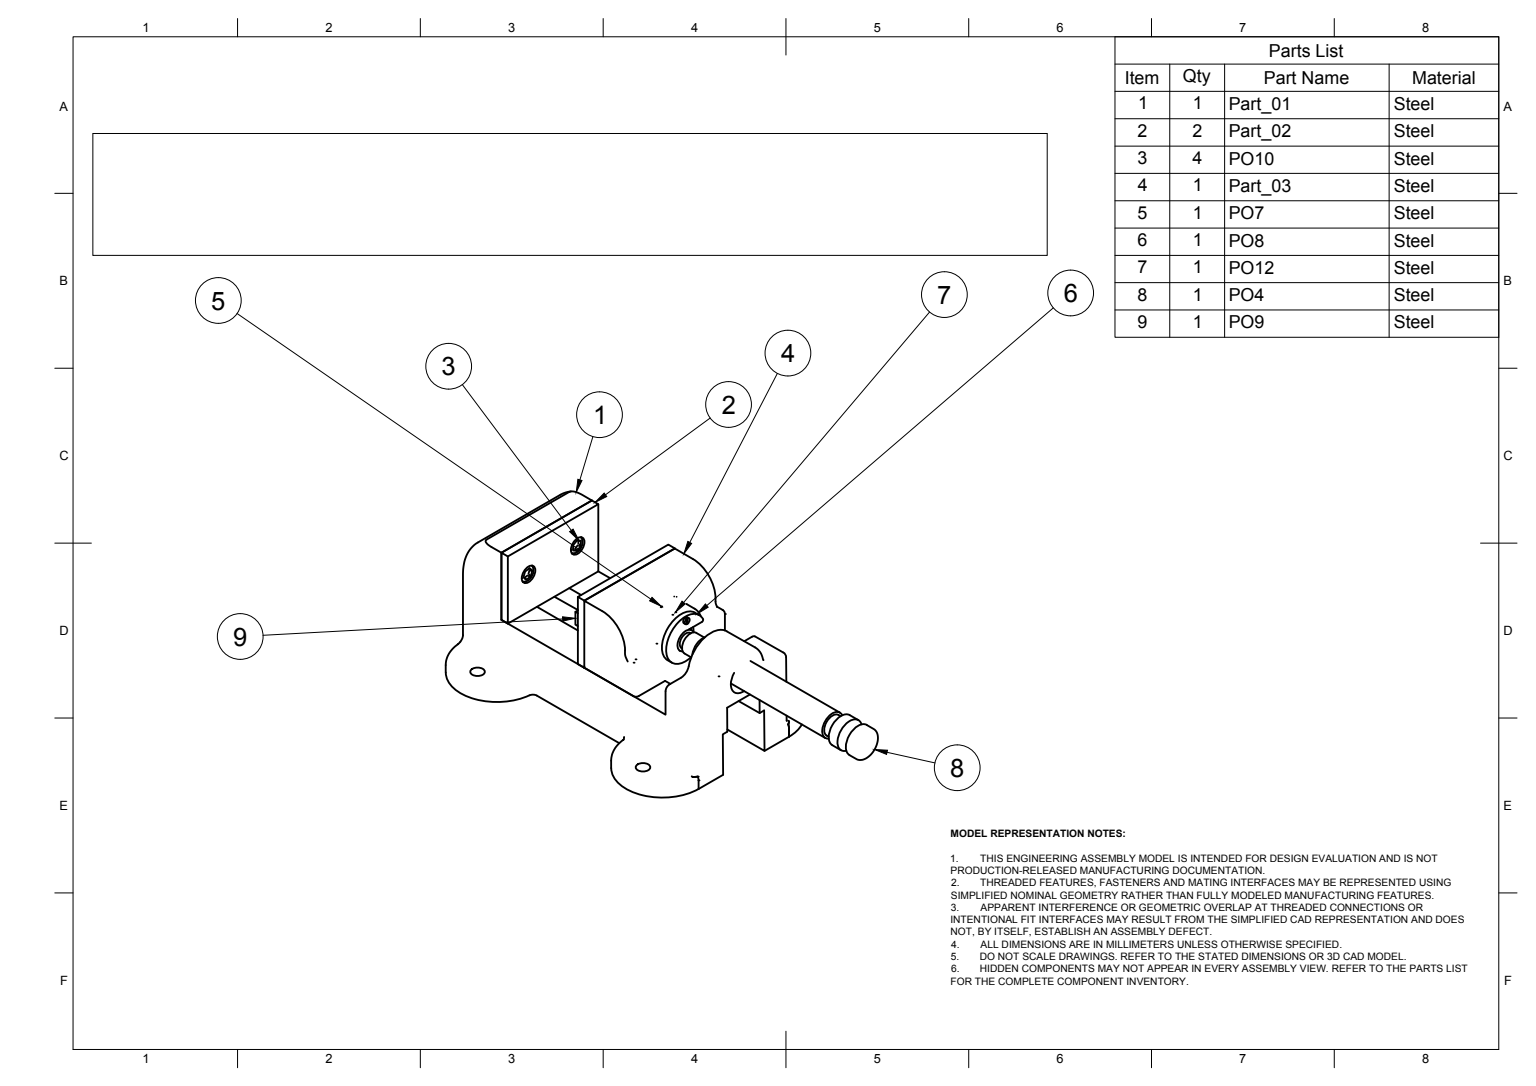
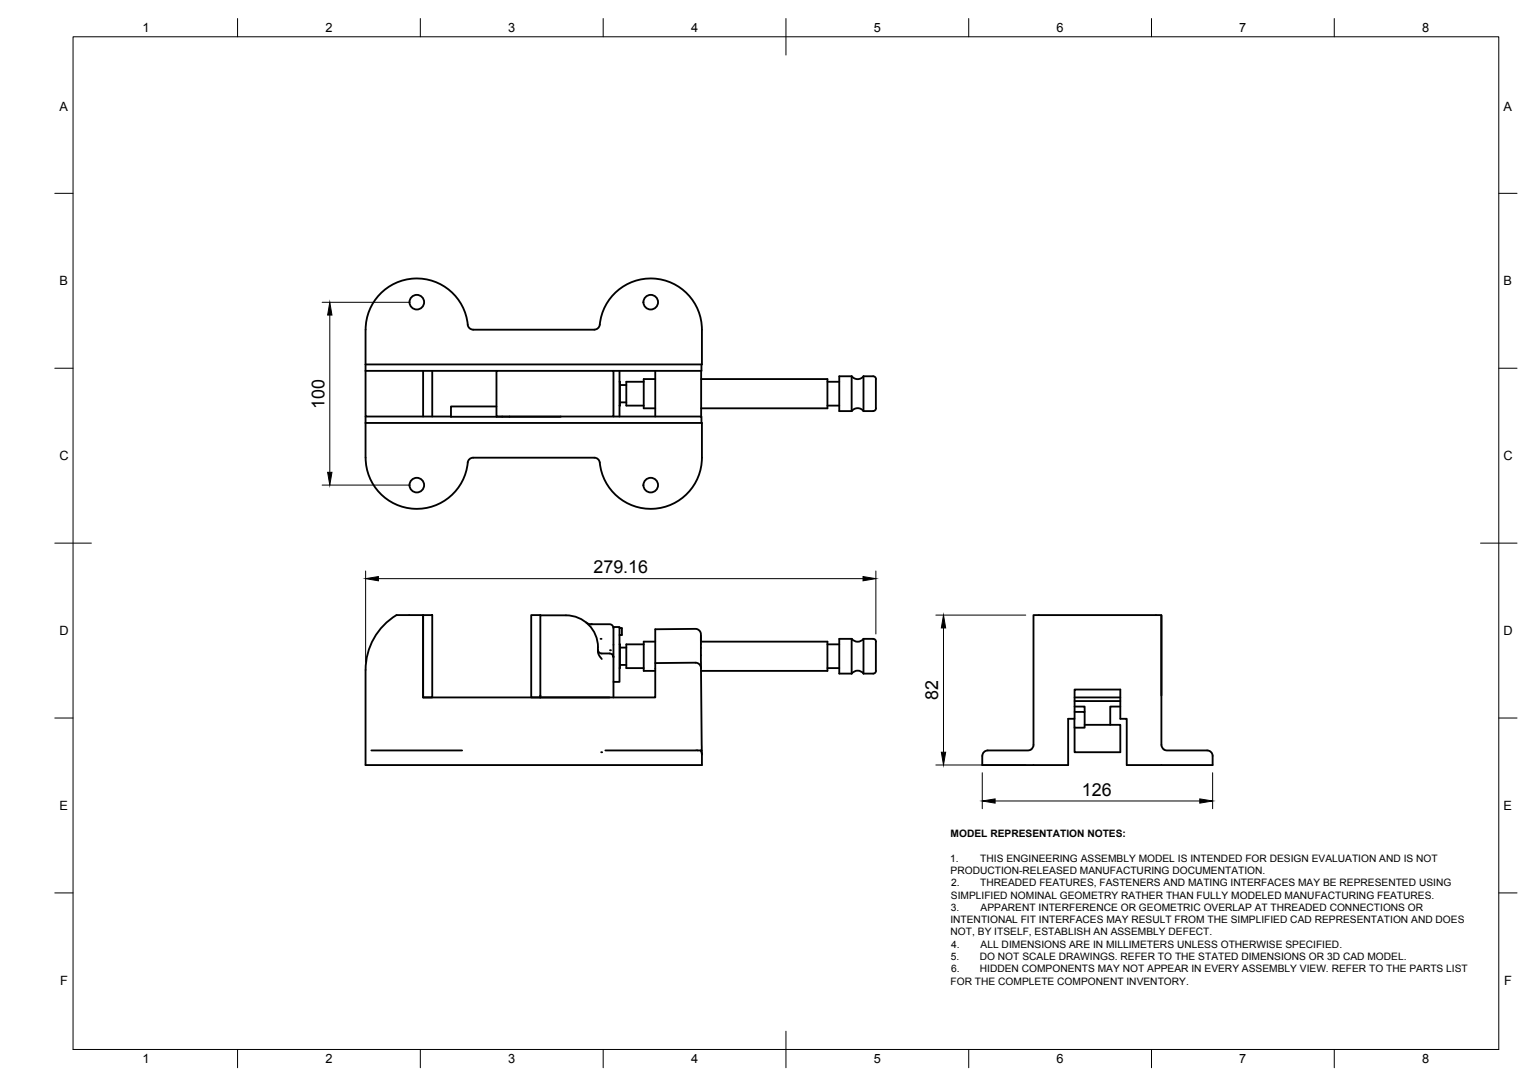
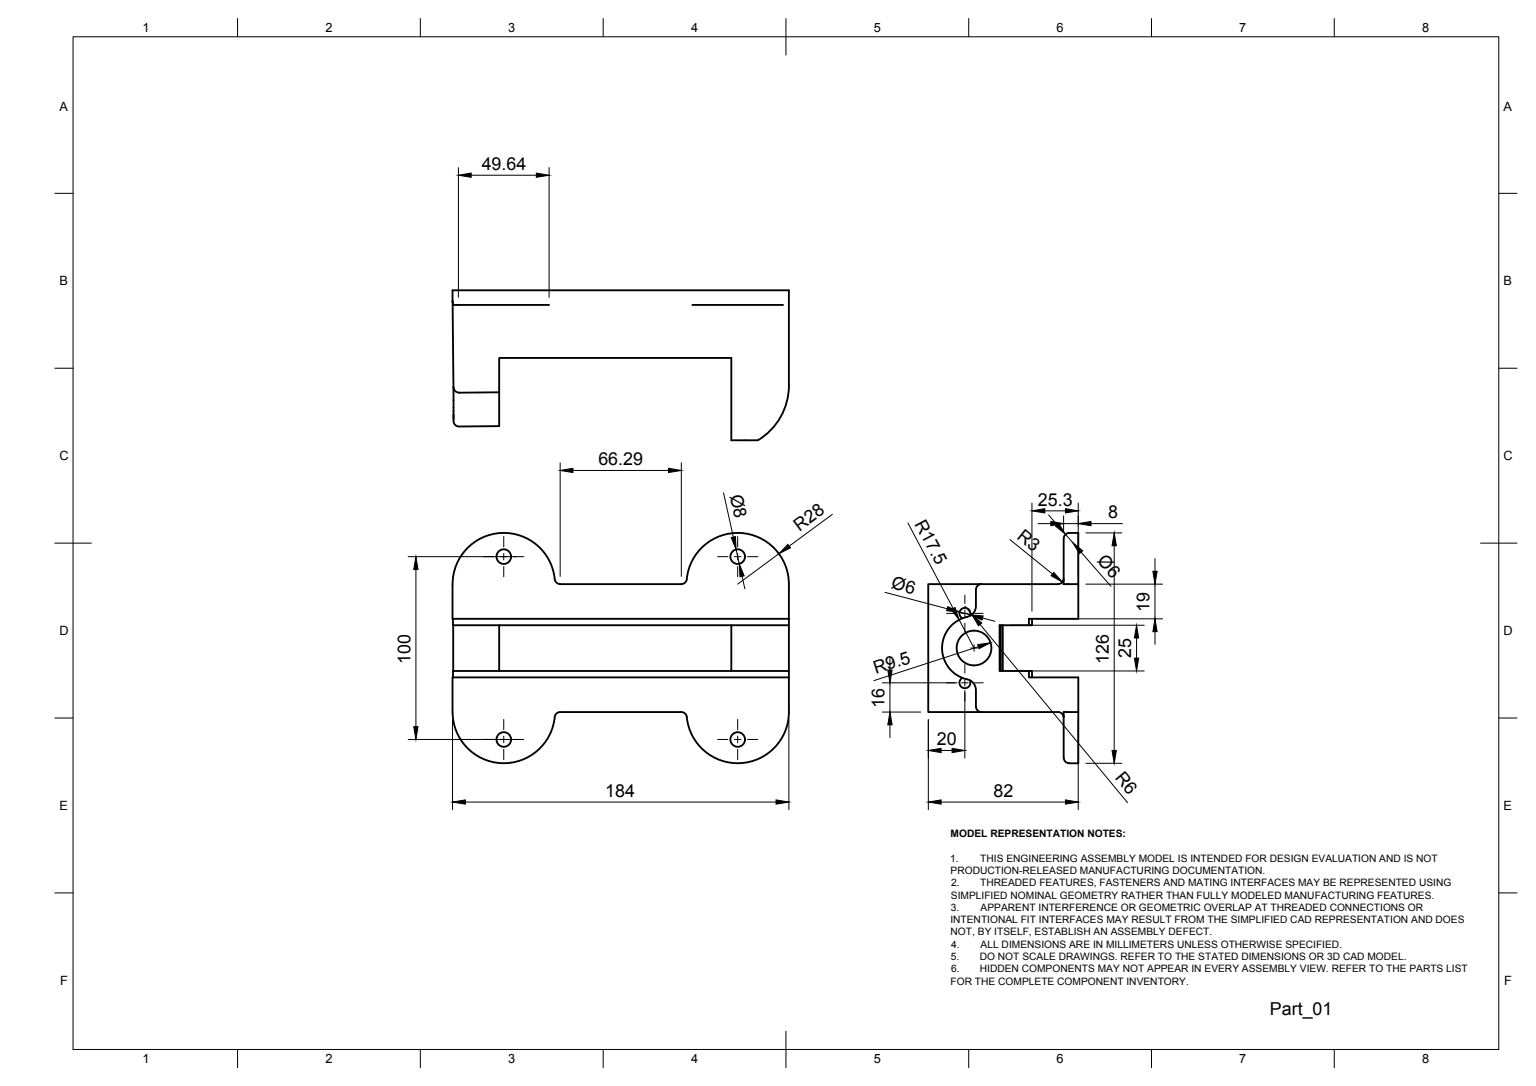
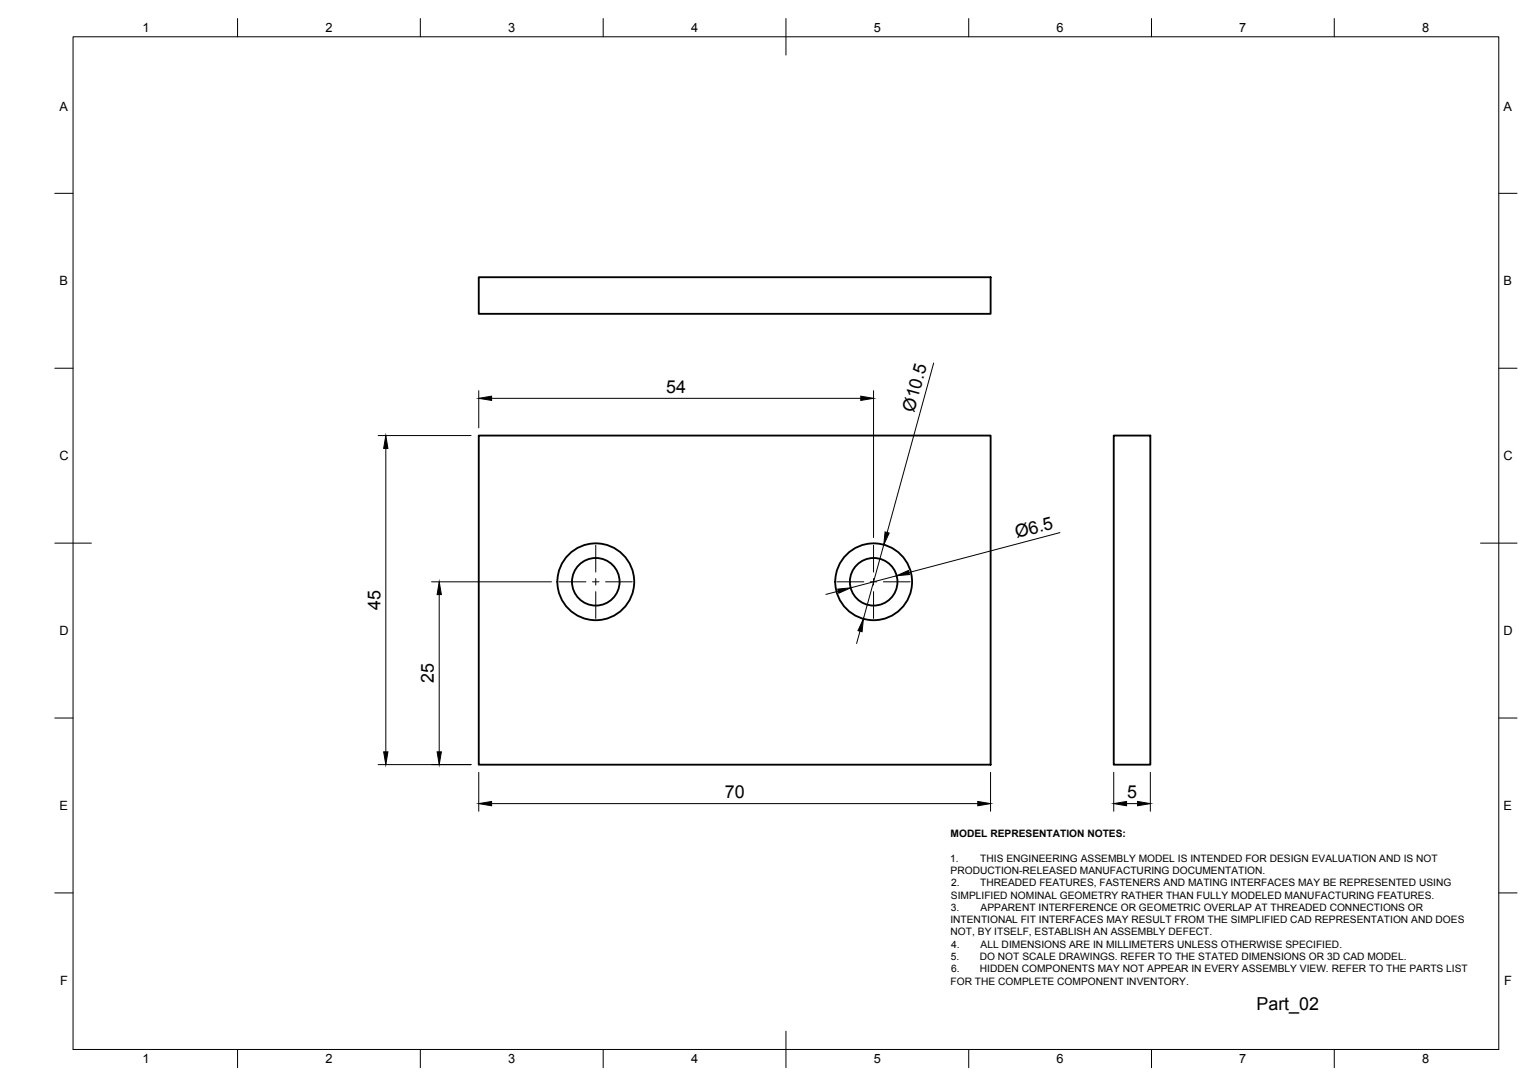
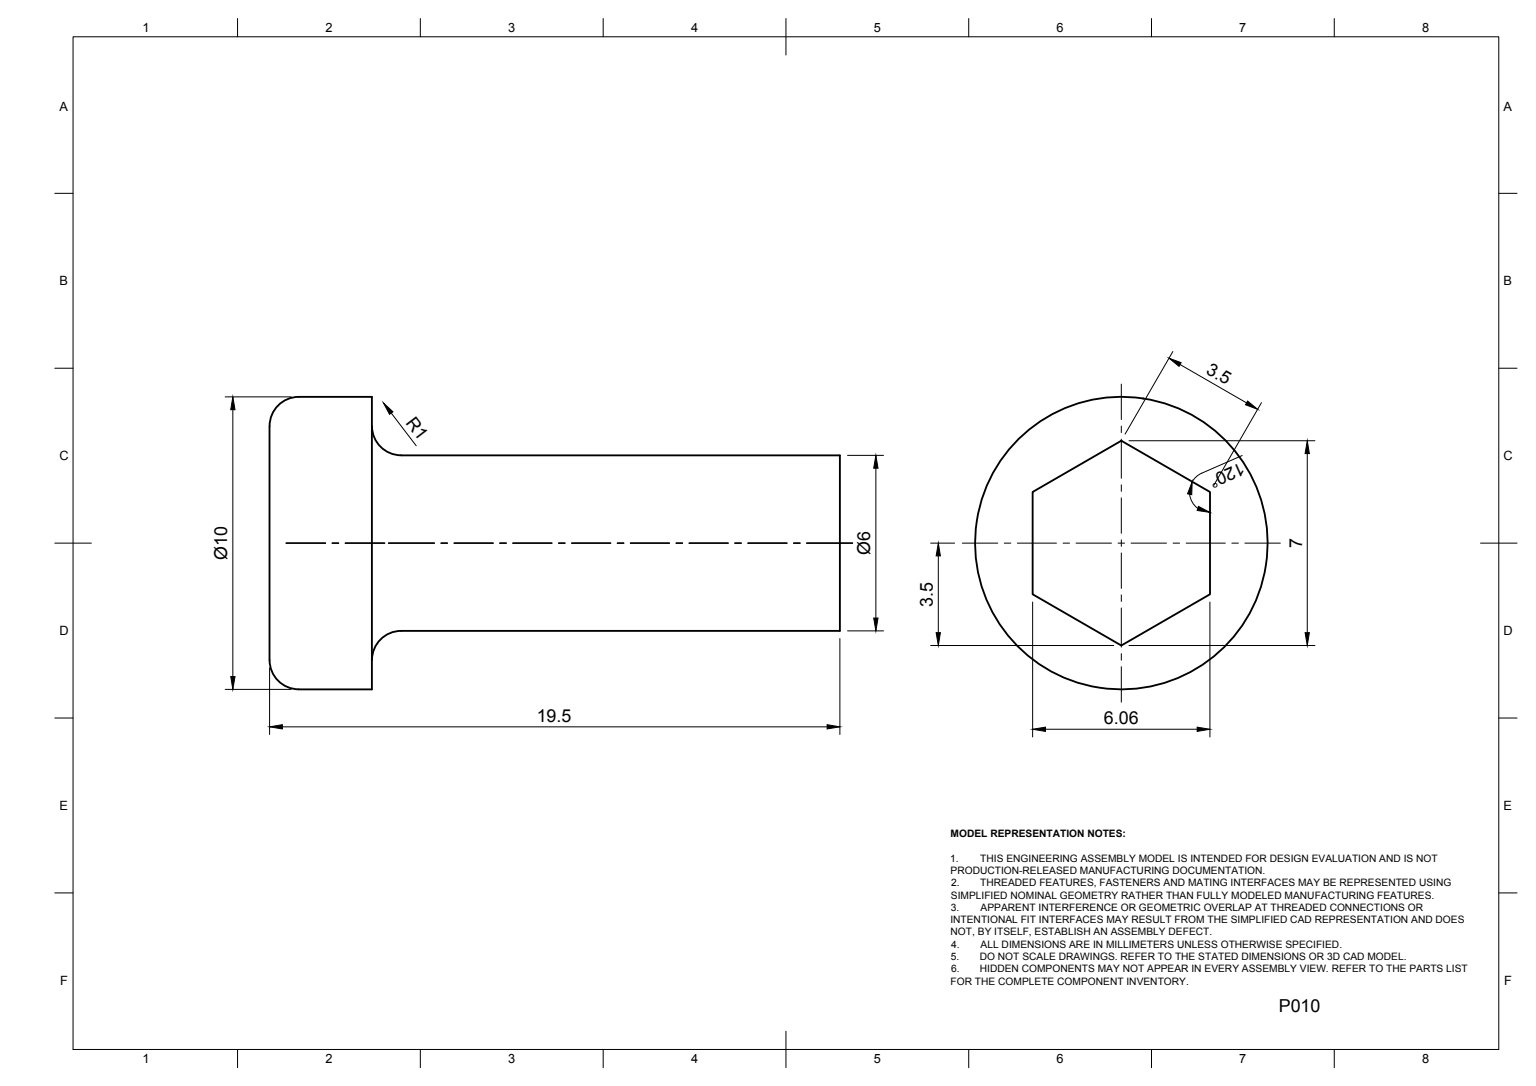
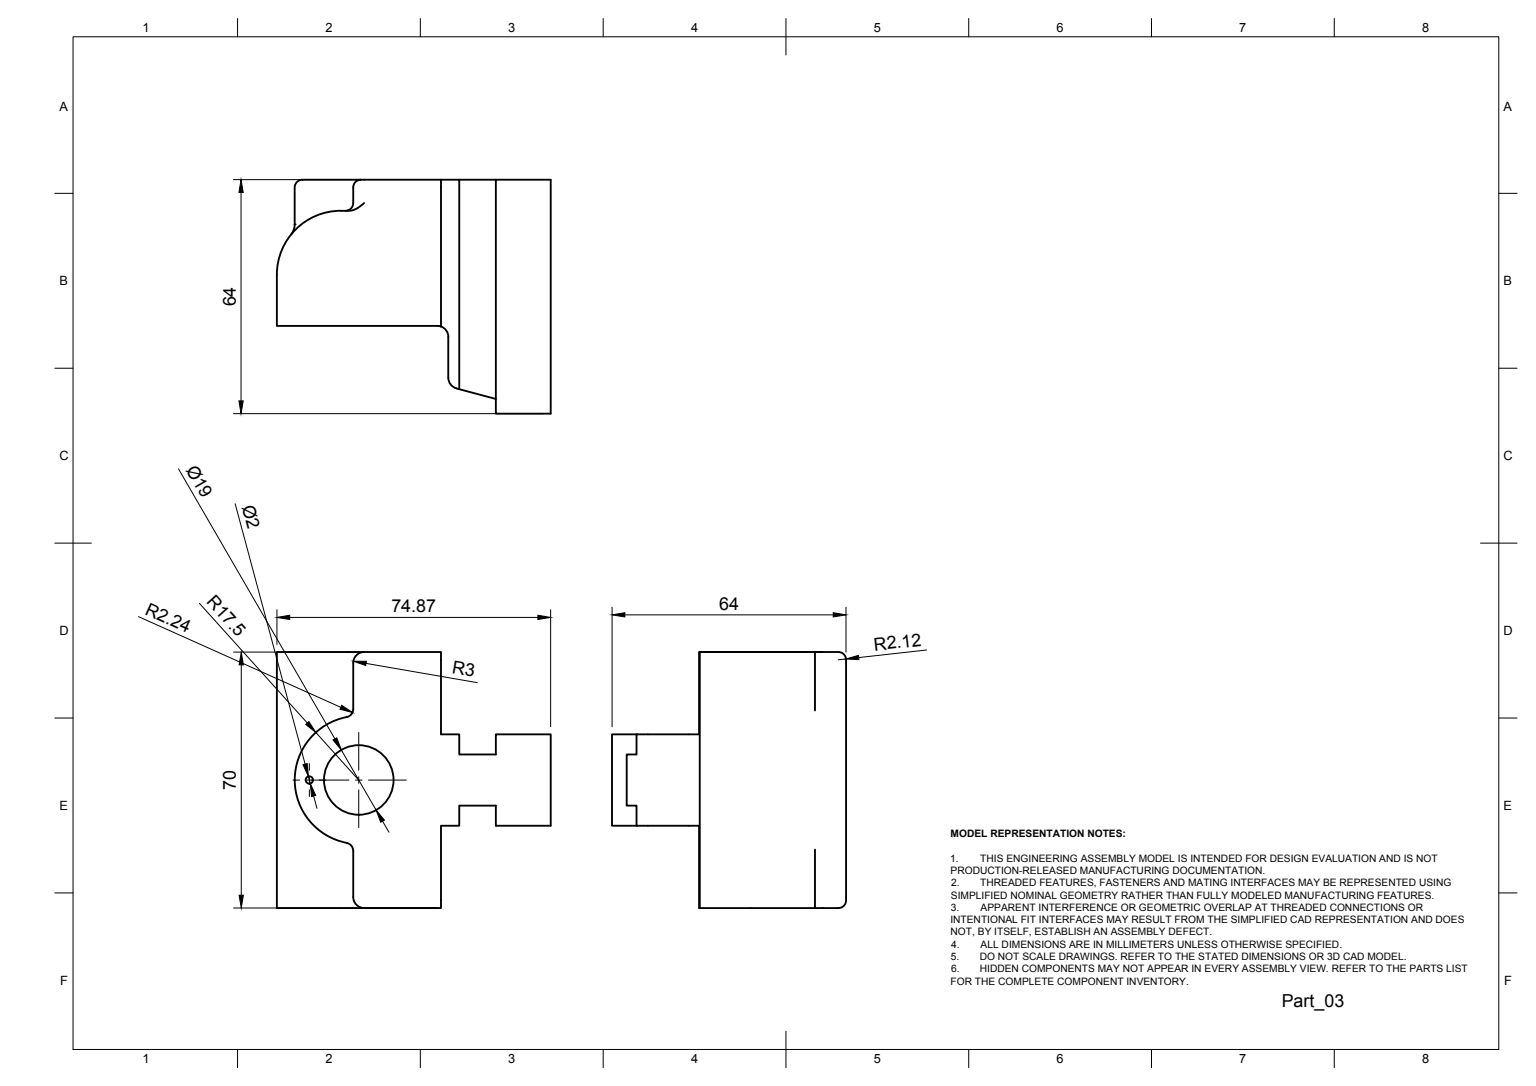
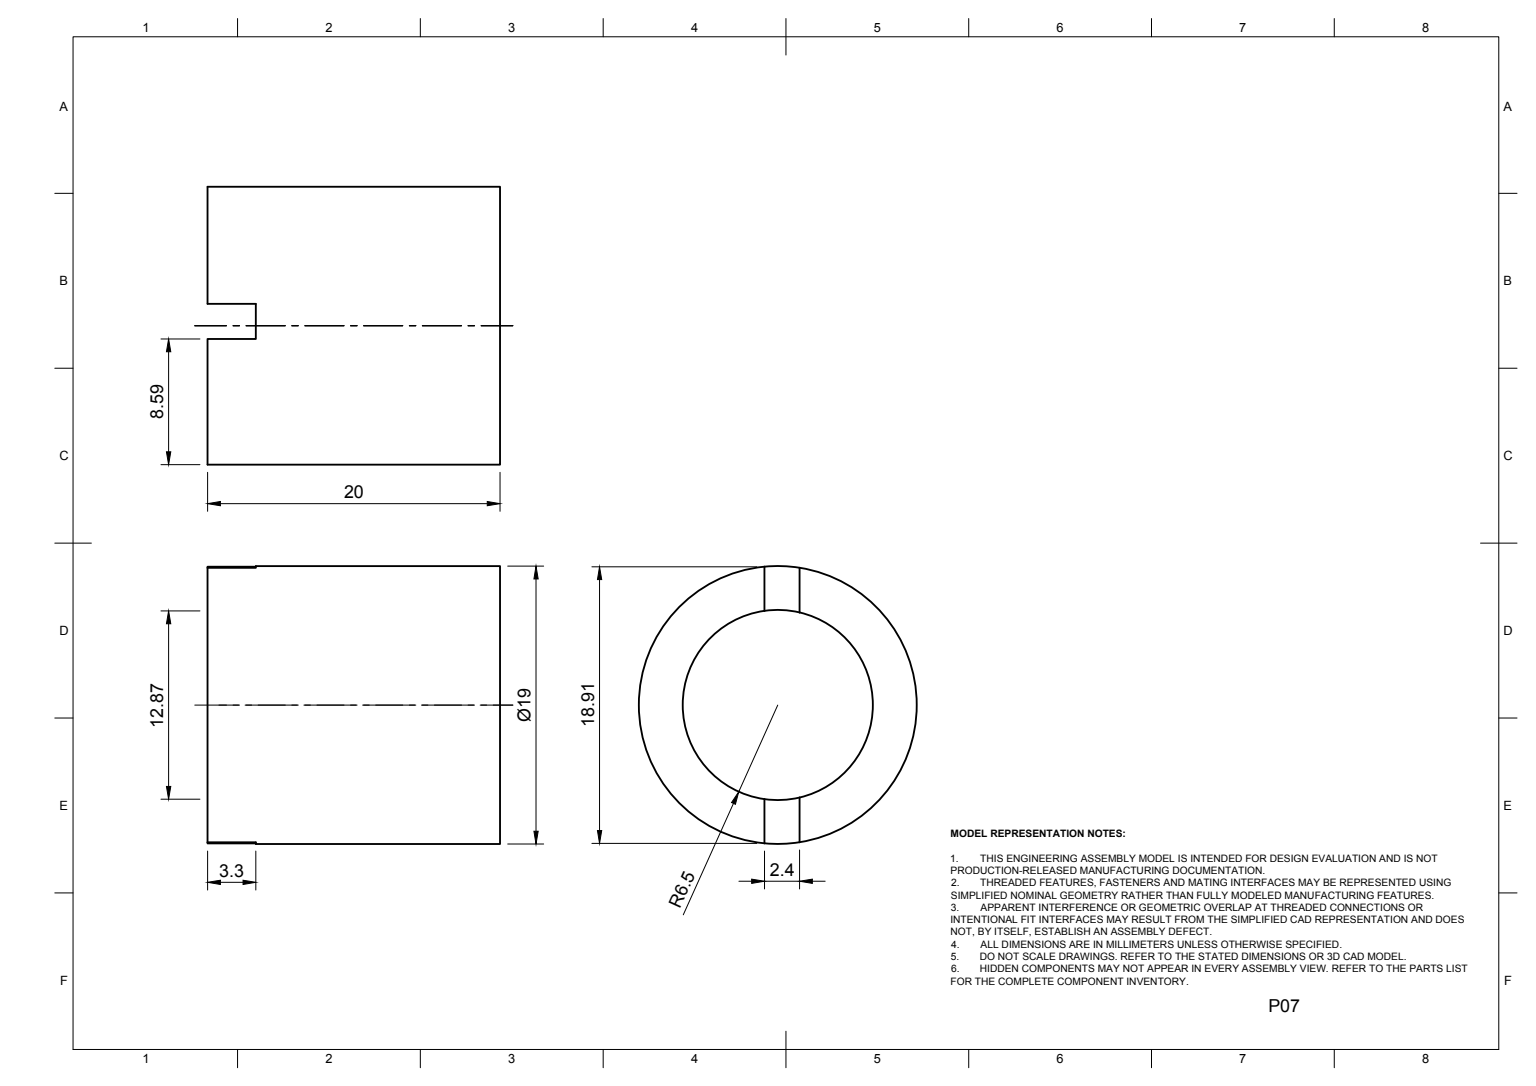
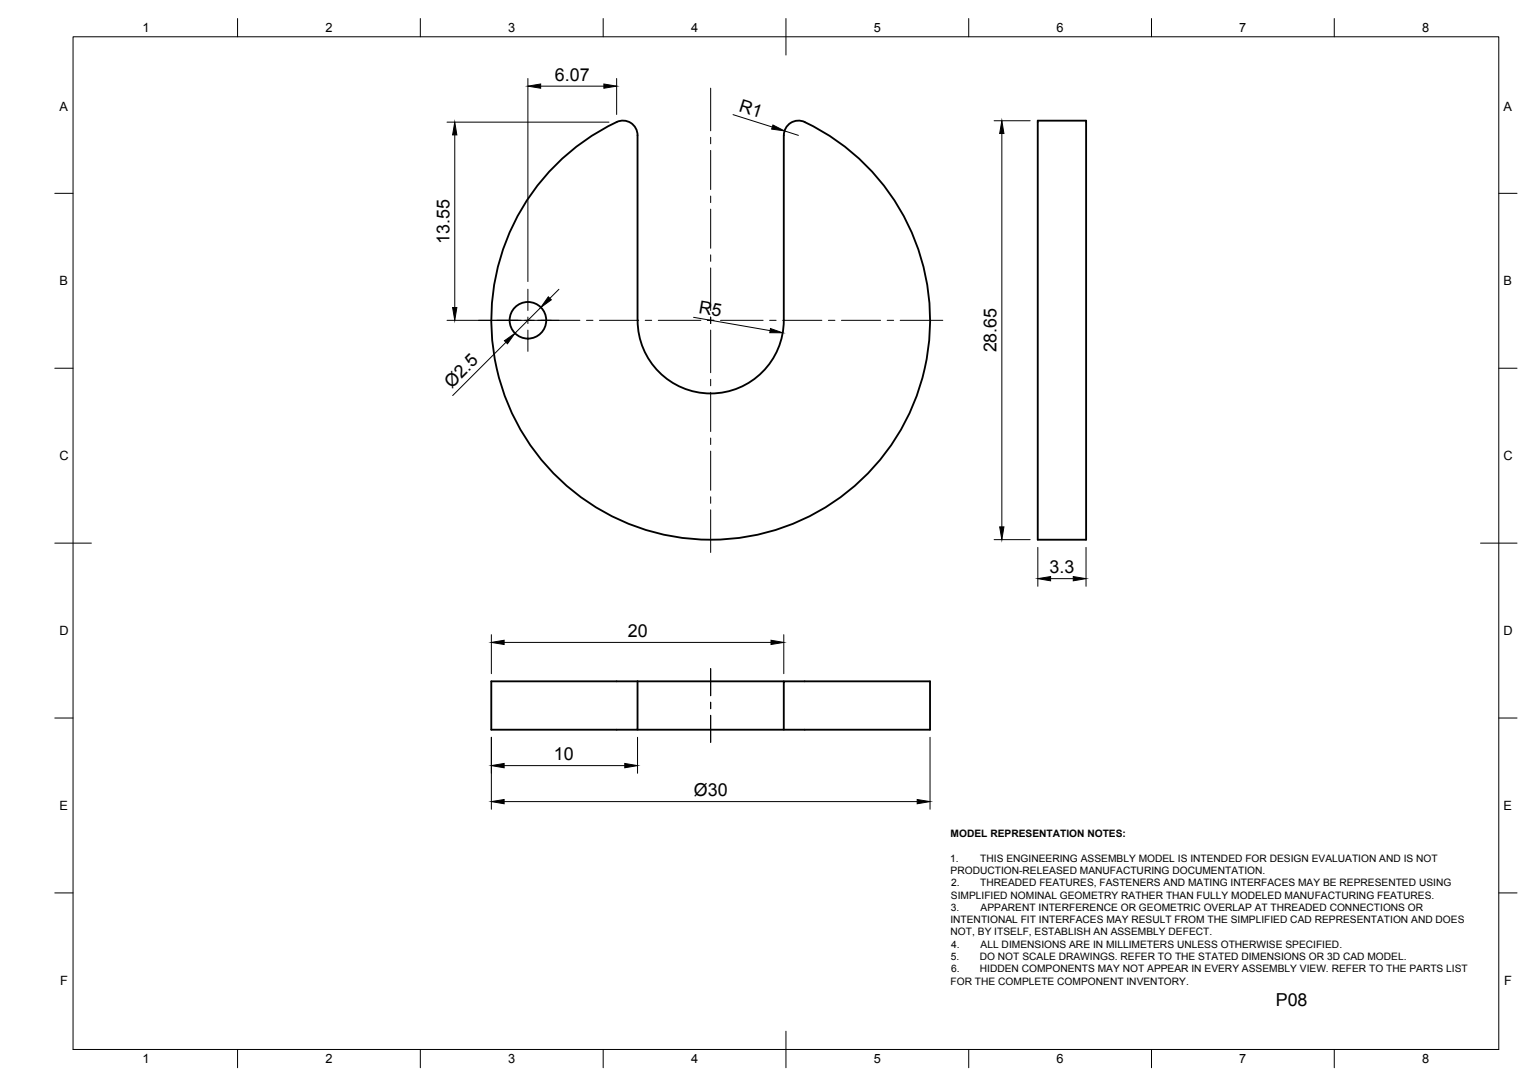
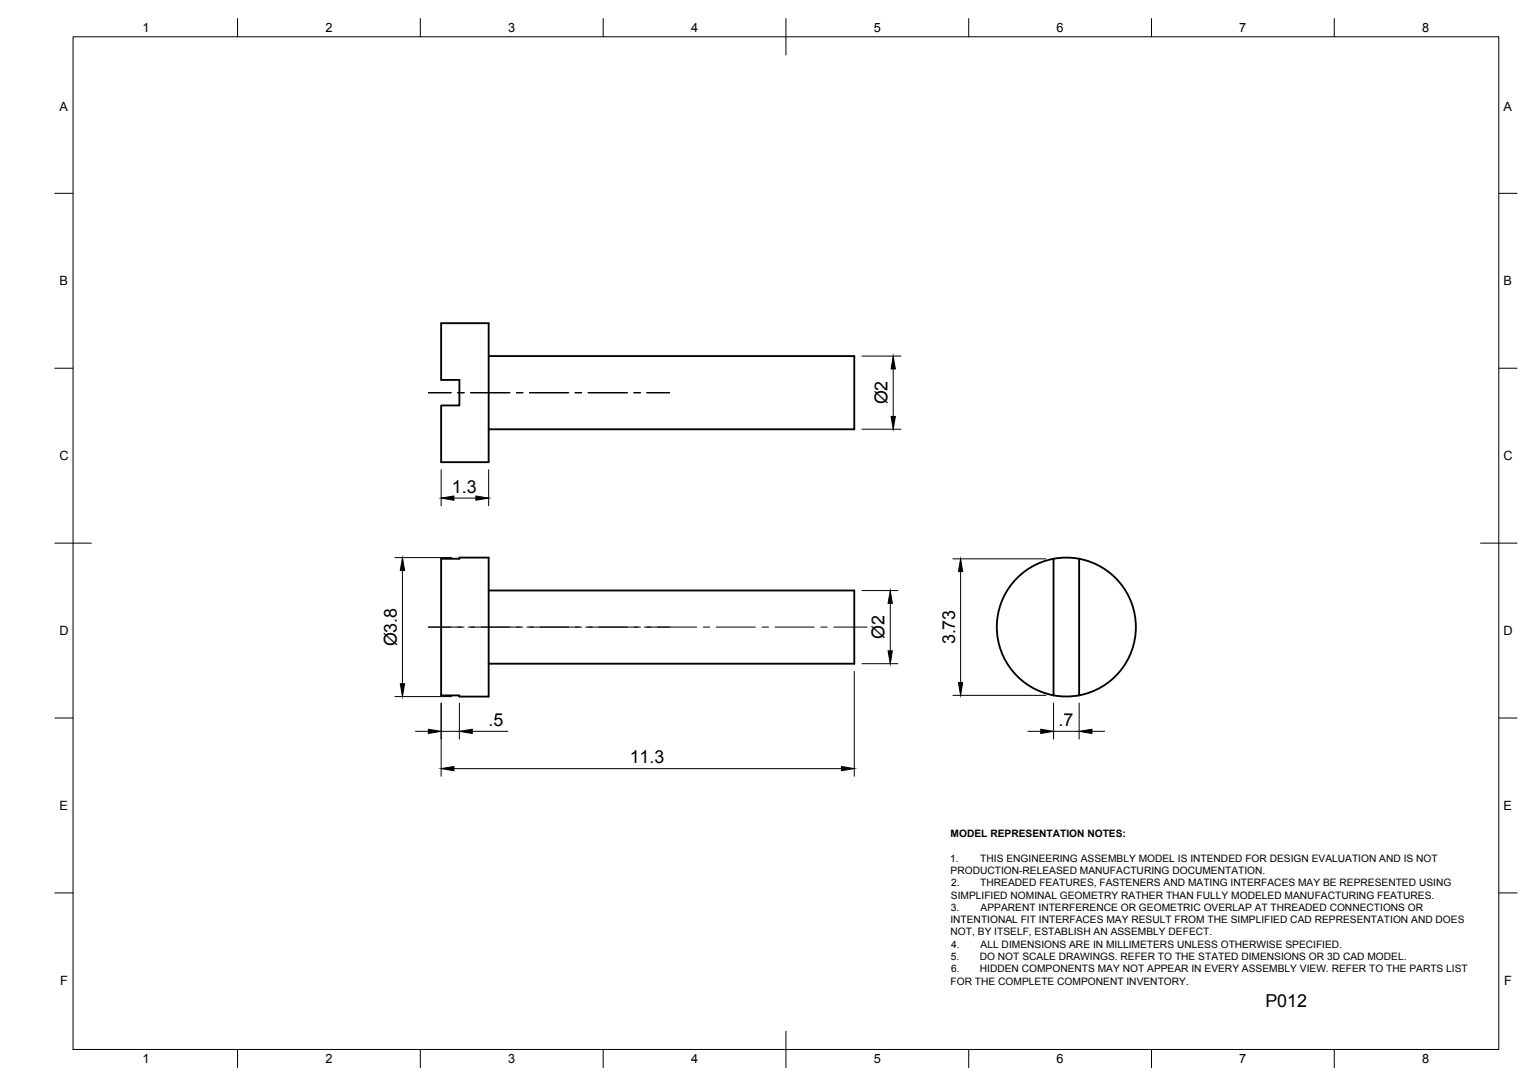
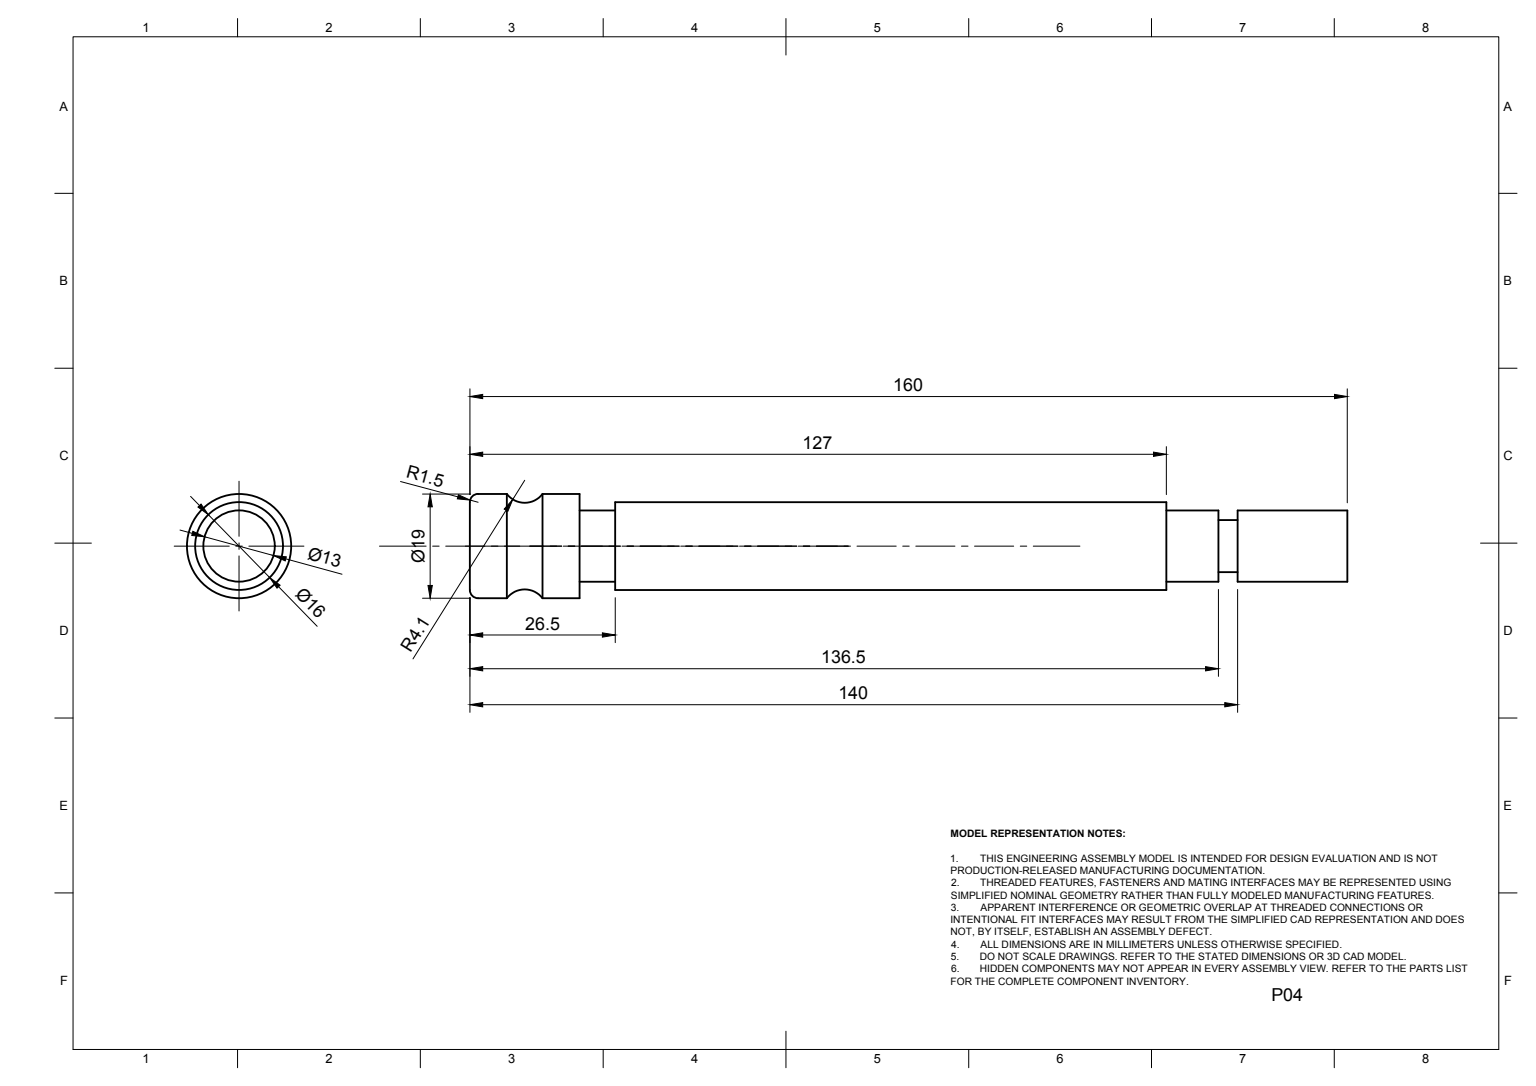
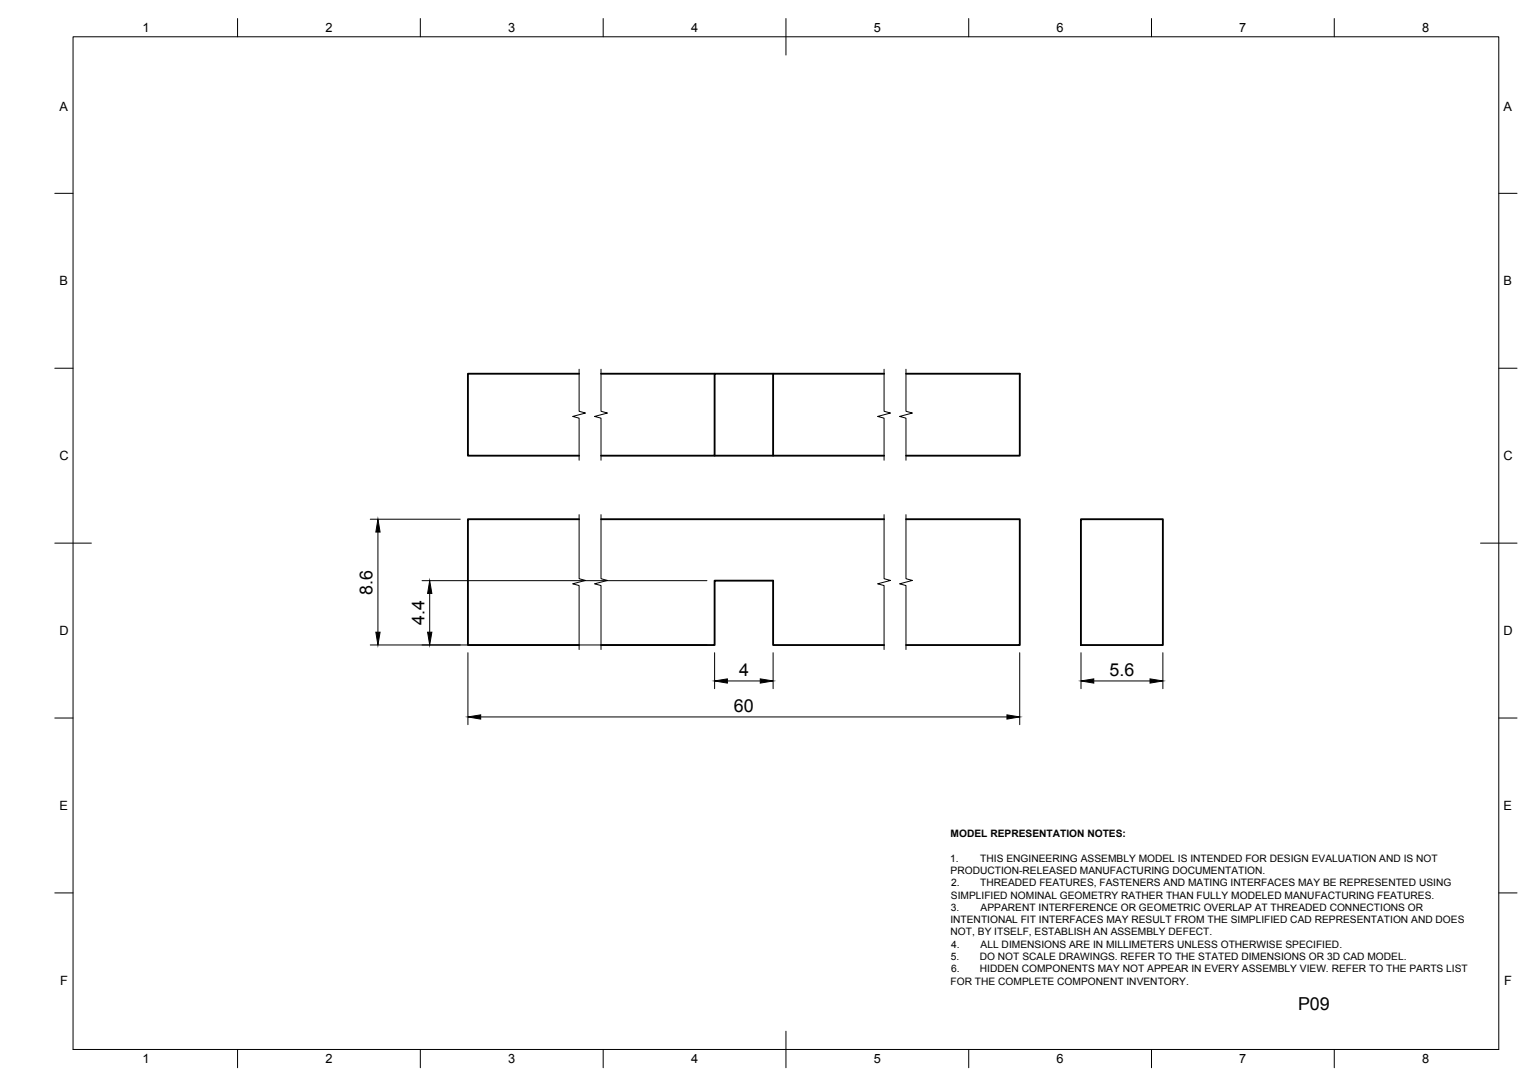
ISO-10303-21;
HEADER;
/* Generated by software containing ST-Developer
 * from STEP Tools, Inc. (www.steptools.com) 
 */

FILE_DESCRIPTION(
/* description */ (''),
/* implementation_level */ '2;1');

FILE_NAME(
/* name */ 'MAS-612',
/* time_stamp */ '2026-10-06T10:18:54-07:00',
/* author */ (''),
/* organization */ (''),
/* preprocessor_version */ 'ST-DEVELOPER v20.2',
/* originating_system */ 'Autodesk Translation Framework v15.15.0.0',
/* authorisation */ '');

FILE_SCHEMA (('AUTOMOTIVE_DESIGN { 1 0 10303 214 3 1 1 }'));
ENDSEC;

DATA;
#10=MECHANICAL_DESIGN_GEOMETRIC_PRESENTATION_REPRESENTATION('',(#81,#82,
#83,#84,#85,#86,#87,#88,#89),#8445);
#11=ITEM_DEFINED_TRANSFORMATION($,$,#4112,#4500);
#12=ITEM_DEFINED_TRANSFORMATION($,$,#4344,#4501);
#13=ITEM_DEFINED_TRANSFORMATION($,$,#4365,#4502);
#14=ITEM_DEFINED_TRANSFORMATION($,$,#4365,#4503);
#15=ITEM_DEFINED_TRANSFORMATION($,$,#4284,#4504);
#16=ITEM_DEFINED_TRANSFORMATION($,$,#4344,#4505);
#17=ITEM_DEFINED_TRANSFORMATION($,$,#4365,#4506);
#18=ITEM_DEFINED_TRANSFORMATION($,$,#4365,#4507);
#19=ITEM_DEFINED_TRANSFORMATION($,$,#4390,#4508);
#20=ITEM_DEFINED_TRANSFORMATION($,$,#4414,#4509);
#21=ITEM_DEFINED_TRANSFORMATION($,$,#4434,#4510);
#22=ITEM_DEFINED_TRANSFORMATION($,$,#4452,#4511);
#23=ITEM_DEFINED_TRANSFORMATION($,$,#4489,#4512);
#24=(
REPRESENTATION_RELATIONSHIP($,$,#8484,#8483)
REPRESENTATION_RELATIONSHIP_WITH_TRANSFORMATION(#11)
SHAPE_REPRESENTATION_RELATIONSHIP()
);
#25=(
REPRESENTATION_RELATIONSHIP($,$,#8486,#8483)
REPRESENTATION_RELATIONSHIP_WITH_TRANSFORMATION(#12)
SHAPE_REPRESENTATION_RELATIONSHIP()
);
#26=(
REPRESENTATION_RELATIONSHIP($,$,#8487,#8483)
REPRESENTATION_RELATIONSHIP_WITH_TRANSFORMATION(#13)
SHAPE_REPRESENTATION_RELATIONSHIP()
);
#27=(
REPRESENTATION_RELATIONSHIP($,$,#8487,#8483)
REPRESENTATION_RELATIONSHIP_WITH_TRANSFORMATION(#14)
SHAPE_REPRESENTATION_RELATIONSHIP()
);
#28=(
REPRESENTATION_RELATIONSHIP($,$,#8485,#8483)
REPRESENTATION_RELATIONSHIP_WITH_TRANSFORMATION(#15)
SHAPE_REPRESENTATION_RELATIONSHIP()
);
#29=(
REPRESENTATION_RELATIONSHIP($,$,#8486,#8483)
REPRESENTATION_RELATIONSHIP_WITH_TRANSFORMATION(#16)
SHAPE_REPRESENTATION_RELATIONSHIP()
);
#30=(
REPRESENTATION_RELATIONSHIP($,$,#8487,#8483)
REPRESENTATION_RELATIONSHIP_WITH_TRANSFORMATION(#17)
SHAPE_REPRESENTATION_RELATIONSHIP()
);
#31=(
REPRESENTATION_RELATIONSHIP($,$,#8487,#8483)
REPRESENTATION_RELATIONSHIP_WITH_TRANSFORMATION(#18)
SHAPE_REPRESENTATION_RELATIONSHIP()
);
#32=(
REPRESENTATION_RELATIONSHIP($,$,#8488,#8483)
REPRESENTATION_RELATIONSHIP_WITH_TRANSFORMATION(#19)
SHAPE_REPRESENTATION_RELATIONSHIP()
);
#33=(
REPRESENTATION_RELATIONSHIP($,$,#8489,#8483)
REPRESENTATION_RELATIONSHIP_WITH_TRANSFORMATION(#20)
SHAPE_REPRESENTATION_RELATIONSHIP()
);
#34=(
REPRESENTATION_RELATIONSHIP($,$,#8490,#8483)
REPRESENTATION_RELATIONSHIP_WITH_TRANSFORMATION(#21)
SHAPE_REPRESENTATION_RELATIONSHIP()
);
#35=(
REPRESENTATION_RELATIONSHIP($,$,#8491,#8483)
REPRESENTATION_RELATIONSHIP_WITH_TRANSFORMATION(#22)
SHAPE_REPRESENTATION_RELATIONSHIP()
);
#36=(
REPRESENTATION_RELATIONSHIP($,$,#8492,#8483)
REPRESENTATION_RELATIONSHIP_WITH_TRANSFORMATION(#23)
SHAPE_REPRESENTATION_RELATIONSHIP()
);
#37=CONTEXT_DEPENDENT_SHAPE_REPRESENTATION(#24,#8470);
#38=CONTEXT_DEPENDENT_SHAPE_REPRESENTATION(#25,#8471);
#39=CONTEXT_DEPENDENT_SHAPE_REPRESENTATION(#26,#8472);
#40=CONTEXT_DEPENDENT_SHAPE_REPRESENTATION(#27,#8473);
#41=CONTEXT_DEPENDENT_SHAPE_REPRESENTATION(#28,#8474);
#42=CONTEXT_DEPENDENT_SHAPE_REPRESENTATION(#29,#8475);
#43=CONTEXT_DEPENDENT_SHAPE_REPRESENTATION(#30,#8476);
#44=CONTEXT_DEPENDENT_SHAPE_REPRESENTATION(#31,#8477);
#45=CONTEXT_DEPENDENT_SHAPE_REPRESENTATION(#32,#8478);
#46=CONTEXT_DEPENDENT_SHAPE_REPRESENTATION(#33,#8479);
#47=CONTEXT_DEPENDENT_SHAPE_REPRESENTATION(#34,#8480);
#48=CONTEXT_DEPENDENT_SHAPE_REPRESENTATION(#35,#8481);
#49=CONTEXT_DEPENDENT_SHAPE_REPRESENTATION(#36,#8482);
#50=NEXT_ASSEMBLY_USAGE_OCCURRENCE('Configuration 1:1',
'Configuration 1:1','Configuration 1:1',#8494,#8495,'Configuration 1:1');
#51=NEXT_ASSEMBLY_USAGE_OCCURRENCE('Configuration 1:1',
'Configuration 1:1','Configuration 1:1',#8494,#8497,'Configuration 1:1');
#52=NEXT_ASSEMBLY_USAGE_OCCURRENCE('PO10:1','PO10:1','PO10:1',#8494,#8498,
'PO10:1');
#53=NEXT_ASSEMBLY_USAGE_OCCURRENCE('PO10:2','PO10:2','PO10:2',#8494,#8498,
'PO10:2');
#54=NEXT_ASSEMBLY_USAGE_OCCURRENCE('Configuration 1:1',
'Configuration 1:1','Configuration 1:1',#8494,#8496,'Configuration 1:1');
#55=NEXT_ASSEMBLY_USAGE_OCCURRENCE('Configuration 1:2',
'Configuration 1:2','Configuration 1:2',#8494,#8497,'Configuration 1:2');
#56=NEXT_ASSEMBLY_USAGE_OCCURRENCE('PO10:3','PO10:3','PO10:3',#8494,#8498,
'PO10:3');
#57=NEXT_ASSEMBLY_USAGE_OCCURRENCE('PO10:4','PO10:4','PO10:4',#8494,#8498,
'PO10:4');
#58=NEXT_ASSEMBLY_USAGE_OCCURRENCE('PO7:1','PO7:1','PO7:1',#8494,#8499,
'PO7:1');
#59=NEXT_ASSEMBLY_USAGE_OCCURRENCE('PO8:1','PO8:1','PO8:1',#8494,#8500,
'PO8:1');
#60=NEXT_ASSEMBLY_USAGE_OCCURRENCE('PO12:1','PO12:1','PO12:1',#8494,#8501,
'PO12:1');
#61=NEXT_ASSEMBLY_USAGE_OCCURRENCE('PO4:1','PO4:1','PO4:1',#8494,#8502,
'PO4:1');
#62=NEXT_ASSEMBLY_USAGE_OCCURRENCE('PO9:1','PO9:1','PO9:1',#8494,#8503,
'PO9:1');
#63=SHAPE_REPRESENTATION_RELATIONSHIP('SRR','None',#8484,#72);
#64=SHAPE_REPRESENTATION_RELATIONSHIP('SRR','None',#8485,#73);
#65=SHAPE_REPRESENTATION_RELATIONSHIP('SRR','None',#8486,#74);
#66=SHAPE_REPRESENTATION_RELATIONSHIP('SRR','None',#8487,#75);
#67=SHAPE_REPRESENTATION_RELATIONSHIP('SRR','None',#8488,#76);
#68=SHAPE_REPRESENTATION_RELATIONSHIP('SRR','None',#8489,#77);
#69=SHAPE_REPRESENTATION_RELATIONSHIP('SRR','None',#8490,#78);
#70=SHAPE_REPRESENTATION_RELATIONSHIP('SRR','None',#8491,#79);
#71=SHAPE_REPRESENTATION_RELATIONSHIP('SRR','None',#8492,#80);
#72=ADVANCED_BREP_SHAPE_REPRESENTATION('',(#90),#8436);
#73=ADVANCED_BREP_SHAPE_REPRESENTATION('',(#91),#8437);
#74=ADVANCED_BREP_SHAPE_REPRESENTATION('',(#92),#8438);
#75=ADVANCED_BREP_SHAPE_REPRESENTATION('',(#93),#8439);
#76=ADVANCED_BREP_SHAPE_REPRESENTATION('',(#94),#8440);
#77=ADVANCED_BREP_SHAPE_REPRESENTATION('',(#95),#8441);
#78=ADVANCED_BREP_SHAPE_REPRESENTATION('',(#96),#8442);
#79=ADVANCED_BREP_SHAPE_REPRESENTATION('',(#97),#8443);
#80=ADVANCED_BREP_SHAPE_REPRESENTATION('',(#98),#8444);
#81=STYLED_ITEM('',(#8537),#90);
#82=STYLED_ITEM('',(#8537),#91);
#83=STYLED_ITEM('',(#8537),#92);
#84=STYLED_ITEM('',(#8537),#93);
#85=STYLED_ITEM('',(#8537),#94);
#86=STYLED_ITEM('',(#8537),#95);
#87=STYLED_ITEM('',(#8537),#96);
#88=STYLED_ITEM('',(#8537),#97);
#89=STYLED_ITEM('',(#8537),#98);
#90=MANIFOLD_SOLID_BREP('Body1',#4002);
#91=MANIFOLD_SOLID_BREP('Body1',#4003);
#92=MANIFOLD_SOLID_BREP('Body1',#4004);
#93=MANIFOLD_SOLID_BREP('Body2',#4005);
#94=MANIFOLD_SOLID_BREP('Body1',#4006);
#95=MANIFOLD_SOLID_BREP('Body1',#4007);
#96=MANIFOLD_SOLID_BREP('Body1',#4008);
#97=MANIFOLD_SOLID_BREP('Body1',#4009);
#98=MANIFOLD_SOLID_BREP('Body1',#4010);
#99=CONICAL_SURFACE('',#4273,1.5,0.523598775598299);
#100=CONICAL_SURFACE('',#4276,1.5,0.523598775598299);
#101=CONICAL_SURFACE('',#4327,0.5,0.872664625997165);
#102=SPHERICAL_SURFACE('',#4234,3.);
#103=SPHERICAL_SURFACE('',#4236,3.);
#104=CYLINDRICAL_SURFACE('',#4148,3.);
#105=CYLINDRICAL_SURFACE('',#4152,3.);
#106=CYLINDRICAL_SURFACE('',#4156,3.);
#107=CYLINDRICAL_SURFACE('',#4162,3.);
#108=CYLINDRICAL_SURFACE('',#4177,3.);
#109=CYLINDRICAL_SURFACE('',#4178,28.);
#110=CYLINDRICAL_SURFACE('',#4187,28.);
#111=CYLINDRICAL_SURFACE('',#4202,3.);
#112=CYLINDRICAL_SURFACE('',#4203,3.);
#113=CYLINDRICAL_SURFACE('',#4210,3.);
#114=CYLINDRICAL_SURFACE('',#4216,3.);
#115=CYLINDRICAL_SURFACE('',#4230,3.);
#116=CYLINDRICAL_SURFACE('',#4232,3.);
#117=CYLINDRICAL_SURFACE('',#4238,28.);
#118=CYLINDRICAL_SURFACE('',#4240,3.);
#119=CYLINDRICAL_SURFACE('',#4243,5.99999999999999);
#120=CYLINDRICAL_SURFACE('',#4245,17.5);
#121=CYLINDRICAL_SURFACE('',#4247,5.99999999999999);
#122=CYLINDRICAL_SURFACE('',#4250,3.);
#123=CYLINDRICAL_SURFACE('',#4254,9.5);
#124=CYLINDRICAL_SURFACE('',#4258,3.);
#125=CYLINDRICAL_SURFACE('',#4260,3.);
#126=CYLINDRICAL_SURFACE('',#4263,3.);
#127=CYLINDRICAL_SURFACE('',#4264,4.);
#128=CYLINDRICAL_SURFACE('',#4266,28.);
#129=CYLINDRICAL_SURFACE('',#4268,4.);
#130=CYLINDRICAL_SURFACE('',#4269,3.99999999999999);
#131=CYLINDRICAL_SURFACE('',#4271,3.99999999999999);
#132=CYLINDRICAL_SURFACE('',#4275,3.);
#133=CYLINDRICAL_SURFACE('',#4278,3.);
#134=CYLINDRICAL_SURFACE('',#4281,35.);
#135=CYLINDRICAL_SURFACE('',#4285,3.);
#136=CYLINDRICAL_SURFACE('',#4289,3.);
#137=CYLINDRICAL_SURFACE('',#4294,17.5);
#138=CYLINDRICAL_SURFACE('',#4300,2.99999999999999);
#139=CYLINDRICAL_SURFACE('',#4302,2.23705055212463);
#140=CYLINDRICAL_SURFACE('',#4303,17.5);
#141=CYLINDRICAL_SURFACE('',#4304,2.23705055212463);
#142=CYLINDRICAL_SURFACE('',#4306,2.99999999999999);
#143=CYLINDRICAL_SURFACE('',#4315,3.00000000000001);
#144=CYLINDRICAL_SURFACE('',#4319,2.99999999999998);
#145=CYLINDRICAL_SURFACE('',#4329,1.);
#146=CYLINDRICAL_SURFACE('',#4331,9.5);
#147=CYLINDRICAL_SURFACE('',#4348,5.25);
#148=CYLINDRICAL_SURFACE('',#4350,3.25);
#149=CYLINDRICAL_SURFACE('',#4355,5.25);
#150=CYLINDRICAL_SURFACE('',#4357,3.25);
#151=CYLINDRICAL_SURFACE('',#4371,3.);
#152=CYLINDRICAL_SURFACE('',#4387,5.);
#153=CYLINDRICAL_SURFACE('',#4409,9.5);
#154=CYLINDRICAL_SURFACE('',#4411,6.5);
#155=CYLINDRICAL_SURFACE('',#4415,1.25);
#156=CYLINDRICAL_SURFACE('',#4418,5.00000007450581);
#157=CYLINDRICAL_SURFACE('',#4422,0.999999999999998);
#158=CYLINDRICAL_SURFACE('',#4425,15.);
#159=CYLINDRICAL_SURFACE('',#4428,1.);
#160=CYLINDRICAL_SURFACE('',#4445,1.);
#161=CYLINDRICAL_SURFACE('',#4449,1.9);
#162=CYLINDRICAL_SURFACE('',#4458,9.5);
#163=CYLINDRICAL_SURFACE('',#4466,9.5);
#164=CYLINDRICAL_SURFACE('',#4470,6.5);
#165=CYLINDRICAL_SURFACE('',#4475,6.50000009685755);
#166=CYLINDRICAL_SURFACE('',#4478,4.75);
#167=CYLINDRICAL_SURFACE('',#4480,6.5);
#168=CYLINDRICAL_SURFACE('',#4484,8.);
#169=ELLIPSE('',#4142,6.70820393249937,3.);
#170=ELLIPSE('',#4143,6.70820393249937,3.);
#171=ELLIPSE('',#4171,6.70820393249937,3.);
#172=ELLIPSE('',#4172,6.70820393249937,3.);
#173=ELLIPSE('',#4180,6.70820393249938,3.);
#174=ELLIPSE('',#4181,6.70820393249937,3.);
#175=ELLIPSE('',#4191,3.00051436158052,3.);
#176=ELLIPSE('',#4193,6.00025719732504,6.);
#177=ELLIPSE('',#4200,6.70820393249937,3.);
#178=ELLIPSE('',#4201,6.70820393249938,3.);
#179=ELLIPSE('',#4204,3.00051436158052,3.);
#180=ELLIPSE('',#4208,6.00025719732504,6.);
#181=ELLIPSE('',#4218,6.0005786784788,5.99999999999999);
#182=ELLIPSE('',#4220,9.00038579598755,8.99999999999999);
#183=ELLIPSE('',#4222,14.5006215602022,14.5);
#184=ELLIPSE('',#4223,17.5005150104847,17.5);
#185=ELLIPSE('',#4224,9.00038579598755,8.99999999999999);
#186=ELLIPSE('',#4225,6.0005786784788,5.99999999999999);
#187=ELLIPSE('',#4241,3.00012859866252,3.);
#188=ELLIPSE('',#4244,6.00025719732503,5.99999999999999);
#189=ELLIPSE('',#4246,17.5007501588647,17.5);
#190=ELLIPSE('',#4248,6.00025719732503,5.99999999999999);
#191=ELLIPSE('',#4251,3.00012859866252,3.);
#192=ELLIPSE('',#4255,9.50040722909798,9.5);
#193=TOROIDAL_SURFACE('',#4137,25.,3.);
#194=TOROIDAL_SURFACE('',#4144,32.,3.);
#195=TOROIDAL_SURFACE('',#4150,6.,3.);
#196=TOROIDAL_SURFACE('',#4158,32.,3.);
#197=TOROIDAL_SURFACE('',#4166,25.,3.);
#198=TOROIDAL_SURFACE('',#4173,6.,3.);
#199=TOROIDAL_SURFACE('',#4183,25.,3.);
#200=TOROIDAL_SURFACE('',#4194,25.,3.);
#201=TOROIDAL_SURFACE('',#4212,8.99999999999999,3.);
#202=TOROIDAL_SURFACE('',#4226,8.99999999999999,3.);
#203=TOROIDAL_SURFACE('',#4366,4.,1.);
#204=TOROIDAL_SURFACE('',#4382,4.,1.);
#205=TOROIDAL_SURFACE('',#4453,8.,1.5);
#206=TOROIDAL_SURFACE('',#4462,12.0000001788139,4.1);
#207=B_SPLINE_CURVE_WITH_KNOTS('',3,(#5747,#5748,#5749,#5750),
 .UNSPECIFIED.,.F.,.F.,(4,4),(-0.314873215025081,0.),.UNSPECIFIED.);
#208=B_SPLINE_CURVE_WITH_KNOTS('',3,(#5753,#5754,#5755,#5756),
 .UNSPECIFIED.,.F.,.F.,(4,4),(0.,0.314873215025081),.UNSPECIFIED.);
#209=B_SPLINE_CURVE_WITH_KNOTS('',3,(#5784,#5785,#5786,#5787),
 .UNSPECIFIED.,.F.,.F.,(4,4),(-0.0585005125063144,0.),.UNSPECIFIED.);
#210=B_SPLINE_CURVE_WITH_KNOTS('',3,(#5790,#5791,#5792,#5793),
 .UNSPECIFIED.,.F.,.F.,(4,4),(0.,0.0585005125063144),.UNSPECIFIED.);
#211=B_SPLINE_CURVE_WITH_KNOTS('',3,(#5835,#5836,#5837,#5838,#5839,#5840,
#5841,#5842,#5843,#5844,#5845,#5846,#5847,#5848),.UNSPECIFIED.,.F.,.F.,
(4,2,2,2,2,2,4),(1.81481027575948,1.85509507173471,1.89964280797494,2.0220220083772,
2.21769356951572,2.39982278968484,2.58195200985395),.UNSPECIFIED.);
#212=B_SPLINE_CURVE_WITH_KNOTS('',3,(#5887,#5888,#5889,#5890,#5891,#5892,
#5893,#5894,#5895,#5896,#5897,#5898,#5899,#5900),.UNSPECIFIED.,.F.,.F.,
(4,2,2,2,2,2,4),(4.67728909318397,4.85941831335309,5.04154753352221,5.23721909466073,
5.35959829506298,5.40414603130322,5.44443082727844),.UNSPECIFIED.);
#213=B_SPLINE_CURVE_WITH_KNOTS('',3,(#5933,#5934,#5935,#5936),
 .UNSPECIFIED.,.F.,.F.,(4,4),(-0.31487081906698,0.),.UNSPECIFIED.);
#214=B_SPLINE_CURVE_WITH_KNOTS('',3,(#5938,#5939,#5940,#5941),
 .UNSPECIFIED.,.F.,.F.,(4,4),(0.,0.31487081906698),.UNSPECIFIED.);
#215=B_SPLINE_CURVE_WITH_KNOTS('',3,(#5971,#5972,#5973,#5974),
 .UNSPECIFIED.,.F.,.F.,(4,4),(-0.0585005125063158,0.),.UNSPECIFIED.);
#216=B_SPLINE_CURVE_WITH_KNOTS('',3,(#5975,#5976,#5977,#5978),
 .UNSPECIFIED.,.F.,.F.,(4,4),(0.,0.0585005125063158),.UNSPECIFIED.);
#217=B_SPLINE_CURVE_WITH_KNOTS('',3,(#6078,#6079,#6080,#6081),
 .UNSPECIFIED.,.F.,.F.,(4,4),(-0.0585005125063147,0.),.UNSPECIFIED.);
#218=B_SPLINE_CURVE_WITH_KNOTS('',3,(#6084,#6085,#6086,#6087),
 .UNSPECIFIED.,.F.,.F.,(4,4),(0.,0.0585005125063147),.UNSPECIFIED.);
#219=B_SPLINE_CURVE_WITH_KNOTS('',3,(#6121,#6122,#6123,#6124,#6125,#6126),
 .UNSPECIFIED.,.F.,.F.,(4,2,4),(0.058804296831916,0.150601760228585,0.290945138364171),
 .UNSPECIFIED.);
#220=B_SPLINE_CURVE_WITH_KNOTS('',3,(#6127,#6128,#6129,#6130,#6131),
 .UNSPECIFIED.,.F.,.F.,(4,1,4),(0.937613435458313,0.988925248429188,1.25041151877174),
 .UNSPECIFIED.);
#221=B_SPLINE_CURVE_WITH_KNOTS('',3,(#6133,#6134,#6135,#6136),
 .UNSPECIFIED.,.F.,.F.,(4,4),(-1.25041151877174,-1.10394303083322),
 .UNSPECIFIED.);
#222=B_SPLINE_CURVE_WITH_KNOTS('',3,(#6138,#6139,#6140,#6141,#6142,#6143),
 .UNSPECIFIED.,.F.,.F.,(4,2,4),(-0.00122772925122373,0.,0.0713282894365937),
 .UNSPECIFIED.);
#223=B_SPLINE_CURVE_WITH_KNOTS('',3,(#6144,#6145,#6146,#6147,#6148,#6149),
 .UNSPECIFIED.,.F.,.F.,(4,2,4),(0.104979741457986,0.218385659282761,0.376958276855987),
 .UNSPECIFIED.);
#224=B_SPLINE_CURVE_WITH_KNOTS('',3,(#6160,#6161,#6162,#6163,#6164,#6165),
 .UNSPECIFIED.,.F.,.F.,(4,2,4),(0.377503618079906,0.433661154495474,0.590536904457044),
 .UNSPECIFIED.);
#225=B_SPLINE_CURVE_WITH_KNOTS('',3,(#6168,#6169,#6170,#6171,#6172,#6173),
 .UNSPECIFIED.,.F.,.F.,(4,2,4),(0.100502924090409,0.233024798286911,0.373363044052317),
 .UNSPECIFIED.);
#226=B_SPLINE_CURVE_WITH_KNOTS('',3,(#6233,#6234,#6235,#6236),
 .UNSPECIFIED.,.F.,.F.,(4,4),(-0.0585005125063158,0.),.UNSPECIFIED.);
#227=B_SPLINE_CURVE_WITH_KNOTS('',3,(#6239,#6240,#6241,#6242),
 .UNSPECIFIED.,.F.,.F.,(4,4),(0.,0.0585005125063158),.UNSPECIFIED.);
#228=B_SPLINE_CURVE_WITH_KNOTS('',3,(#6303,#6304,#6305,#6306,#6307,#6308,
#6309,#6310,#6311,#6312,#6313,#6314,#6315),.UNSPECIFIED.,.F.,.F.,(4,3,3,
3,4),(0.395698154007737,0.425905162440753,0.455555657972498,0.466932501158666,
0.468163517607288),.UNSPECIFIED.);
#229=B_SPLINE_CURVE_WITH_KNOTS('',3,(#6316,#6317,#6318,#6319),
 .UNSPECIFIED.,.F.,.F.,(4,4),(1.10577580098667,1.25278641295821),
 .UNSPECIFIED.);
#230=B_SPLINE_CURVE_WITH_KNOTS('',3,(#6321,#6322,#6323,#6324),
 .UNSPECIFIED.,.F.,.F.,(4,4),(-1.25278641295821,-0.938561283624521),
 .UNSPECIFIED.);
#231=B_SPLINE_CURVE_WITH_KNOTS('',3,(#6326,#6327,#6328,#6329,#6330,#6331),
 .UNSPECIFIED.,.F.,.F.,(4,2,4),(0.,0.139148474445525,0.230280439948345),
 .UNSPECIFIED.);
#232=B_SPLINE_CURVE_WITH_KNOTS('',3,(#6332,#6333,#6334,#6335,#6336,#6337),
 .UNSPECIFIED.,.F.,.F.,(4,2,4),(0.0496921589401031,0.160922541821051,0.240485355391862),
 .UNSPECIFIED.);
#233=B_SPLINE_CURVE_WITH_KNOTS('',3,(#6349,#6350,#6351,#6352,#6353,#6354),
 .UNSPECIFIED.,.F.,.F.,(4,2,4),(0.195057093979392,0.323802001349606,0.445376130695255),
 .UNSPECIFIED.);
#234=B_SPLINE_CURVE_WITH_KNOTS('',3,(#6384,#6385,#6386,#6387,#6388,#6389),
 .UNSPECIFIED.,.F.,.F.,(4,2,4),(0.,0.143083785469884,0.194304148687177),
 .UNSPECIFIED.);
#235=B_SPLINE_CURVE_WITH_KNOTS('',3,(#6407,#6408,#6409,#6410,#6411,#6412,
#6413,#6414,#6415,#6416,#6417,#6418),.UNSPECIFIED.,.F.,.F.,(4,2,2,2,2,4),
(-0.0021944909380558,0.,0.118954781425746,0.236148568198992,0.353341240908116,
0.470533846489538),.UNSPECIFIED.);
#236=B_SPLINE_CURVE_WITH_KNOTS('',3,(#6451,#6452,#6453,#6454,#6455,#6456,
#6457),.UNSPECIFIED.,.F.,.F.,(4,3,4),(-0.537933556304323,-0.536871151957347,
-0.536116003149211),.UNSPECIFIED.);
#237=B_SPLINE_CURVE_WITH_KNOTS('',3,(#6538,#6539,#6540,#6541,#6542,#6543,
#6544,#6545,#6546,#6547,#6548,#6549,#6550,#6551,#6552,#6553,#6554,#6555,
#6556,#6557,#6558,#6559,#6560,#6561,#6562,#6563,#6564,#6565,#6566,#6567,
#6568,#6569,#6570,#6571,#6572,#6573,#6574,#6575,#6576,#6577,#6578,#6579,
#6580,#6581,#6582,#6583,#6584,#6585,#6586,#6587,#6588,#6589,#6590,#6591,
#6592),.UNSPECIFIED.,.F.,.F.,(4,3,3,3,3,3,3,3,3,3,3,3,3,3,3,3,3,3,4),(-0.472728188530224,
-0.470533698488276,-0.440746367412676,-0.410416837256165,-0.379701952247477,
-0.351578951638149,-0.320921325925665,-0.290206141350092,-0.260036055125886,
-0.234385204179885,-0.203800840065922,-0.201744974296049,-0.171564828698904,
-0.141015529658378,-0.117192569025982,-0.0867072980072964,-0.0561496264825006,
-0.0261504853702348,0.),.UNSPECIFIED.);
#238=B_SPLINE_CURVE_WITH_KNOTS('',3,(#6593,#6594,#6595,#6596,#6597,#6598,
#6599),.UNSPECIFIED.,.F.,.F.,(4,3,4),(-0.00165554359406403,-0.00116998025873546,
0.),.UNSPECIFIED.);
#239=B_SPLINE_CURVE_WITH_KNOTS('',3,(#6764,#6765,#6766,#6767,#6768,#6769,
#6770),.UNSPECIFIED.,.F.,.F.,(4,1,1,1,4),(-1.,-0.785714285714286,-0.571428571428571,
-0.285714285714286,0.),.UNSPECIFIED.);
#240=B_SPLINE_CURVE_WITH_KNOTS('',3,(#6772,#6773,#6774,#6775,#6776),
 .UNSPECIFIED.,.F.,.F.,(4,1,4),(-0.801055439138956,-0.45774596523445,-2.84420950871177E-11),
 .UNSPECIFIED.);
#241=B_SPLINE_CURVE_WITH_KNOTS('',3,(#6778,#6779,#6780,#6781,#6782,#6783,
#6784,#6785,#6786,#6787,#6788,#6789,#6790,#6791,#6792,#6793,#6794,#6795,
#6796,#6797,#6798,#6799,#6800,#6801),.UNSPECIFIED.,.F.,.F.,(4,2,2,2,2,2,
2,2,2,2,2,4),(0.,0.000472673310068606,0.00105992669792163,0.00191515129472927,
0.00337317925368863,0.00606809230516856,0.0123496565483333,0.0257034558078238,
0.0532576217839337,0.110508433799565,0.205819736498927,0.232965615027244),
 .UNSPECIFIED.);
#242=B_SPLINE_CURVE_WITH_KNOTS('',3,(#6802,#6803,#6804,#6805),
 .UNSPECIFIED.,.F.,.F.,(4,4),(0.480969105510275,0.801055439138956),
 .UNSPECIFIED.);
#243=B_SPLINE_CURVE_WITH_KNOTS('',3,(#6836,#6837,#6838,#6839,#6840,#6841,
#6842),.UNSPECIFIED.,.F.,.F.,(4,1,1,1,4),(-1.,-0.785714285714286,-0.571428571428571,
-0.285714285714286,0.),.UNSPECIFIED.);
#244=B_SPLINE_CURVE_WITH_KNOTS('',3,(#6843,#6844,#6845,#6846),
 .UNSPECIFIED.,.F.,.F.,(4,4),(-2.06290888015454,-0.801055439138956),
 .UNSPECIFIED.);
#245=B_SPLINE_CURVE_WITH_KNOTS('',3,(#6847,#6848,#6849,#6850),
 .UNSPECIFIED.,.F.,.F.,(4,4),(0.801055439138956,2.06290888015454),
 .UNSPECIFIED.);
#246=B_SPLINE_CURVE_WITH_KNOTS('',3,(#6888,#6889,#6890,#6891,#6892,#6893,
#6894),.UNSPECIFIED.,.F.,.F.,(4,1,1,1,4),(-1.,-0.785714285714286,-0.571428571428571,
-0.285714285714286,0.),.UNSPECIFIED.);
#247=B_SPLINE_CURVE_WITH_KNOTS('',3,(#6895,#6896,#6897,#6898,#6899),
 .UNSPECIFIED.,.F.,.F.,(4,1,4),(-2.07918288771298,-2.069883451706,-2.06290887470076),
 .UNSPECIFIED.);
#248=B_SPLINE_CURVE_WITH_KNOTS('',3,(#6900,#6901,#6902,#6903,#6904),
 .UNSPECIFIED.,.F.,.F.,(4,1,4),(2.06290888015454,2.069883451706,2.07918288771298),
 .UNSPECIFIED.);
#249=B_SPLINE_CURVE_WITH_KNOTS('',3,(#6935,#6936,#6937,#6938,#6939,#6940,
#6941),.UNSPECIFIED.,.F.,.F.,(4,1,1,1,4),(-1.,-0.785714285714286,-0.571428571428571,
-0.285714285714286,0.),.UNSPECIFIED.);
#250=B_SPLINE_CURVE_WITH_KNOTS('',3,(#6942,#6943,#6944,#6945),
 .UNSPECIFIED.,.F.,.F.,(4,4),(-2.19760564616015,-2.07918288771299),
 .UNSPECIFIED.);
#251=B_SPLINE_CURVE_WITH_KNOTS('',3,(#6946,#6947,#6948,#6949),
 .UNSPECIFIED.,.F.,.F.,(4,4),(2.07918288771299,2.19760564616015),
 .UNSPECIFIED.);
#252=B_SPLINE_CURVE_WITH_KNOTS('',3,(#7036,#7037,#7038,#7039,#7040,#7041,
#7042),.UNSPECIFIED.,.F.,.F.,(4,1,1,1,4),(-1.,-0.785714285714286,-0.571428571428571,
-0.285714285714286,0.),.UNSPECIFIED.);
#253=B_SPLINE_CURVE_WITH_KNOTS('',3,(#7043,#7044,#7045,#7046,#7047,#7048,
#7049,#7050,#7051,#7052,#7053,#7054),.UNSPECIFIED.,.F.,.F.,(4,1,1,1,1,1,
1,1,1,4),(-7.78726759776434,-6.98874446182879,-6.19022132589323,-5.39169818995768,
-4.85934943266731,-4.59317505402212,-4.32700067537694,-3.79465191808657,
-2.99612878215101,-2.19760564621546),.UNSPECIFIED.);
#254=B_SPLINE_CURVE_WITH_KNOTS('',3,(#7055,#7056,#7057,#7058,#7059,#7060,
#7061,#7062,#7063,#7064,#7065,#7066),.UNSPECIFIED.,.F.,.F.,(4,1,1,1,1,1,
1,1,1,4),(2.19760564621546,2.99612878215101,3.79465191808657,4.32700067537694,
4.59317505402212,4.85934943266731,5.39169818995768,6.19022132589323,6.98874446182879,
7.78726759776434),.UNSPECIFIED.);
#255=B_SPLINE_CURVE_WITH_KNOTS('',3,(#7097,#7098,#7099,#7100,#7101,#7102,
#7103),.UNSPECIFIED.,.F.,.F.,(4,1,1,1,4),(-1.,-0.785714285714286,-0.571428571428571,
-0.285714285714286,0.),.UNSPECIFIED.);
#256=B_SPLINE_CURVE_WITH_KNOTS('',3,(#7104,#7105,#7106,#7107),
 .UNSPECIFIED.,.F.,.F.,(4,4),(-7.9056903551329,-7.78726759776434),
 .UNSPECIFIED.);
#257=B_SPLINE_CURVE_WITH_KNOTS('',3,(#7108,#7109,#7110,#7111),
 .UNSPECIFIED.,.F.,.F.,(4,4),(7.78726759776434,7.9056903551329),
 .UNSPECIFIED.);
#258=B_SPLINE_CURVE_WITH_KNOTS('',3,(#7149,#7150,#7151,#7152,#7153,#7154,
#7155),.UNSPECIFIED.,.F.,.F.,(4,1,1,1,4),(-1.,-0.785714285714286,-0.571428571428571,
-0.285714285714286,0.),.UNSPECIFIED.);
#259=B_SPLINE_CURVE_WITH_KNOTS('',3,(#7156,#7157,#7158,#7159,#7160),
 .UNSPECIFIED.,.F.,.F.,(4,1,4),(-7.92196437367001,-7.91266493450595,-7.90569035513291),
 .UNSPECIFIED.);
#260=B_SPLINE_CURVE_WITH_KNOTS('',3,(#7161,#7162,#7163,#7164,#7165),
 .UNSPECIFIED.,.F.,.F.,(4,1,4),(7.90569035513291,7.91266493450595,7.92196437367001),
 .UNSPECIFIED.);
#261=B_SPLINE_CURVE_WITH_KNOTS('',3,(#7196,#7197,#7198,#7199,#7200,#7201,
#7202),.UNSPECIFIED.,.F.,.F.,(4,1,1,1,4),(-1.,-0.785714285714286,-0.571428571428571,
-0.285714285714286,0.),.UNSPECIFIED.);
#262=B_SPLINE_CURVE_WITH_KNOTS('',3,(#7203,#7204,#7205,#7206),
 .UNSPECIFIED.,.F.,.F.,(4,4),(-9.18381780243075,-7.92196436821623),
 .UNSPECIFIED.);
#263=B_SPLINE_CURVE_WITH_KNOTS('',3,(#7207,#7208,#7209,#7210),
 .UNSPECIFIED.,.F.,.F.,(4,4),(7.92196437367001,9.18381780243075),
 .UNSPECIFIED.);
#264=B_SPLINE_CURVE_WITH_KNOTS('',3,(#7241,#7242,#7243,#7244,#7245,#7246,
#7247),.UNSPECIFIED.,.F.,.F.,(4,1,1,1,4),(-1.,-0.785714285714286,-0.571428571428571,
-0.285714285714286,0.),.UNSPECIFIED.);
#265=B_SPLINE_CURVE_WITH_KNOTS('',3,(#7248,#7249,#7250,#7251),
 .UNSPECIFIED.,.F.,.F.,(4,4),(-9.50411765280707,-9.18381780243075),
 .UNSPECIFIED.);
#266=B_SPLINE_CURVE_WITH_KNOTS('',3,(#7252,#7253,#7254,#7255),
 .UNSPECIFIED.,.F.,.F.,(4,4),(9.18381780243075,9.50411765280707),
 .UNSPECIFIED.);
#267=B_SPLINE_CURVE_WITH_KNOTS('',3,(#7292,#7293,#7294,#7295,#7296,#7297,
#7298,#7299,#7300,#7301,#7302,#7303,#7304,#7305,#7306,#7307,#7308,#7309),
 .UNSPECIFIED.,.F.,.F.,(4,2,2,2,2,2,2,2,4),(0.,0.106887180350865,0.224851448313138,
0.271289364363703,0.289291419641123,0.316349671609722,0.338485570421449,
0.344422245486414,0.347293667204052),.UNSPECIFIED.);
#268=B_SPLINE_CURVE_WITH_KNOTS('',3,(#7311,#7312,#7313,#7314),
 .UNSPECIFIED.,.F.,.F.,(4,4),(-0.00685019644261114,0.),.UNSPECIFIED.);
#269=B_SPLINE_CURVE_WITH_KNOTS('',3,(#7315,#7316,#7317,#7318,#7319),
 .UNSPECIFIED.,.F.,.F.,(4,1,4),(-9.98769942445863,-9.71136698388339,-9.50411765345197),
 .UNSPECIFIED.);
#270=B_SPLINE_CURVE_WITH_KNOTS('',3,(#7339,#7340,#7341,#7342),
 .UNSPECIFIED.,.F.,.F.,(4,4),(-11.987699095758,-9.98769942445863),
 .UNSPECIFIED.);
#271=B_SPLINE_CURVE_WITH_KNOTS('',3,(#7343,#7344,#7345,#7346,#7347,#7348),
 .UNSPECIFIED.,.F.,.F.,(4,2,4),(0.,1.27049294037848,2.00000006501177),
 .UNSPECIFIED.);
#272=B_SPLINE_CURVE_WITH_KNOTS('',3,(#7393,#7394,#7395,#7396,#7397,#7398,
#7399,#7400,#7401,#7402,#7403,#7404,#7405),.UNSPECIFIED.,.F.,.F.,(4,3,3,
3,4),(0.,0.0716322252392672,0.143264450478534,0.238774084130891,0.334283717783247),
 .UNSPECIFIED.);
#273=B_SPLINE_CURVE_WITH_KNOTS('',3,(#7407,#7408,#7409,#7410),
 .UNSPECIFIED.,.F.,.F.,(4,4),(-12.4397849599923,-10.3397956275468),
 .UNSPECIFIED.);
#274=B_SPLINE_CURVE_WITH_KNOTS('',3,(#7412,#7413,#7414,#7415,#7416,#7417,
#7418),.UNSPECIFIED.,.F.,.F.,(4,1,1,1,4),(0.,0.285714285714286,0.571428571428571,
0.785714285714286,1.),.UNSPECIFIED.);
#275=B_SPLINE_CURVE_WITH_KNOTS('',3,(#7419,#7420,#7421,#7422),
 .UNSPECIFIED.,.F.,.F.,(4,4),(10.3397956275468,12.4397849599923),
 .UNSPECIFIED.);
#276=B_SPLINE_CURVE_WITH_KNOTS('',3,(#7460,#7461,#7462,#7463,#7464,#7465,
#7466),.UNSPECIFIED.,.F.,.F.,(4,1,1,1,4),(-1.,-0.785714285714286,-0.571428571428571,
-0.285714285714286,0.),.UNSPECIFIED.);
#277=B_SPLINE_CURVE_WITH_KNOTS('',3,(#7467,#7468,#7469,#7470,#7471),
 .UNSPECIFIED.,.F.,.F.,(4,1,4),(10.2018503099656,10.2806762057263,10.3397956275468),
 .UNSPECIFIED.);
#278=B_SPLINE_CURVE_WITH_KNOTS('',3,(#7472,#7473,#7474,#7475,#7476),
 .UNSPECIFIED.,.F.,.F.,(4,1,4),(-10.3397956275468,-10.2806762057263,-10.2018503099656),
 .UNSPECIFIED.);
#279=B_SPLINE_CURVE_WITH_KNOTS('',3,(#7507,#7508,#7509,#7510,#7511,#7512,
#7513),.UNSPECIFIED.,.F.,.F.,(4,1,1,1,4),(0.,0.285714285714286,0.571428571428571,
0.785714285714286,1.),.UNSPECIFIED.);
#280=B_SPLINE_CURVE_WITH_KNOTS('',3,(#7514,#7515,#7516,#7517),
 .UNSPECIFIED.,.F.,.F.,(4,4),(8.93986452633385,10.2018503099635),
 .UNSPECIFIED.);
#281=B_SPLINE_CURVE_WITH_KNOTS('',3,(#7518,#7519,#7520,#7521),
 .UNSPECIFIED.,.F.,.F.,(4,4),(-10.2018503099635,-8.93986452633385),
 .UNSPECIFIED.);
#282=B_SPLINE_CURVE_WITH_KNOTS('',3,(#7559,#7560,#7561,#7562,#7563,#7564,
#7565),.UNSPECIFIED.,.F.,.F.,(4,1,1,1,4),(0.,0.285714285714286,0.571428571428571,
0.785714285714286,1.),.UNSPECIFIED.);
#283=B_SPLINE_CURVE_WITH_KNOTS('',3,(#7566,#7567,#7568,#7569,#7570),
 .UNSPECIFIED.,.F.,.F.,(4,1,4),(8.33860637357674,8.68218245774598,8.93986452087291),
 .UNSPECIFIED.);
#284=B_SPLINE_CURVE_WITH_KNOTS('',3,(#7571,#7572,#7573,#7574,#7575),
 .UNSPECIFIED.,.F.,.F.,(4,1,4),(-8.93986451541198,-8.68218245774598,-8.33860637357674),
 .UNSPECIFIED.);
#285=B_SPLINE_CURVE_WITH_KNOTS('',3,(#7648,#7649,#7650,#7651,#7652,#7653,
#7654),.UNSPECIFIED.,.F.,.F.,(4,1,1,1,4),(-1.,-0.785714285714286,-0.571428571428571,
-0.285714285714286,0.),.UNSPECIFIED.);
#286=B_SPLINE_CURVE_WITH_KNOTS('',3,(#7655,#7656,#7657,#7658,#7659,#7660,
#7661,#7662,#7663,#7664),.UNSPECIFIED.,.F.,.F.,(4,1,1,1,1,1,1,4),(4.10117860516752,
4.7065253970806,5.31187222649662,5.91721905591265,6.52256588532867,7.12791271474469,
7.73325954416072,8.33860637357674),.UNSPECIFIED.);
#287=B_SPLINE_CURVE_WITH_KNOTS('',3,(#7665,#7666,#7667,#7668,#7669,#7670,
#7671,#7672,#7673,#7674),.UNSPECIFIED.,.F.,.F.,(4,1,1,1,1,1,1,4),(-8.33860637357674,
-7.73325954416072,-7.12791271474469,-6.52256588532867,-5.91721905591265,
-5.31187222649662,-4.7065253970806,-4.10117860516752),.UNSPECIFIED.);
#288=B_SPLINE_CURVE_WITH_KNOTS('',3,(#7712,#7713,#7714,#7715,#7716,#7717,
#7718),.UNSPECIFIED.,.F.,.F.,(4,1,1,1,4),(0.,0.285714285714286,0.571428571428571,
0.785714285714286,1.),.UNSPECIFIED.);
#289=B_SPLINE_CURVE_WITH_KNOTS('',3,(#7719,#7720,#7721,#7722,#7723),
 .UNSPECIFIED.,.F.,.F.,(4,1,4),(3.4999204445805,3.75760250536717,4.10117858641605),
 .UNSPECIFIED.);
#290=B_SPLINE_CURVE_WITH_KNOTS('',3,(#7724,#7725,#7726,#7727,#7728),
 .UNSPECIFIED.,.F.,.F.,(4,1,4),(-4.10117858641605,-3.75760250536717,-3.4999204445805),
 .UNSPECIFIED.);
#291=B_SPLINE_CURVE_WITH_KNOTS('',3,(#7759,#7760,#7761,#7762,#7763,#7764,
#7765),.UNSPECIFIED.,.F.,.F.,(4,1,1,1,4),(-1.,-0.785714285714286,-0.571428571428571,
-0.285714285714286,0.),.UNSPECIFIED.);
#292=B_SPLINE_CURVE_WITH_KNOTS('',3,(#7766,#7767,#7768,#7769),
 .UNSPECIFIED.,.F.,.F.,(4,4),(2.23793465002183,3.49992043911957),
 .UNSPECIFIED.);
#293=B_SPLINE_CURVE_WITH_KNOTS('',3,(#7770,#7771,#7772,#7773),
 .UNSPECIFIED.,.F.,.F.,(4,4),(-3.49992043365863,-2.23793465002183),
 .UNSPECIFIED.);
#294=B_SPLINE_CURVE_WITH_KNOTS('',3,(#7811,#7812,#7813,#7814,#7815,#7816,
#7817),.UNSPECIFIED.,.F.,.F.,(4,1,1,1,4),(-1.,-0.785714285714286,-0.571428571428571,
-0.285714285714286,0.),.UNSPECIFIED.);
#295=B_SPLINE_CURVE_WITH_KNOTS('',3,(#7818,#7819,#7820,#7821,#7822),
 .UNSPECIFIED.,.F.,.F.,(4,1,4),(2.09998933244391,2.17881522820334,2.23793465002292),
 .UNSPECIFIED.);
#296=B_SPLINE_CURVE_WITH_KNOTS('',3,(#7823,#7824,#7825,#7826,#7827),
 .UNSPECIFIED.,.F.,.F.,(4,1,4),(-2.23793465002292,-2.17881522820334,-2.09998933244391),
 .UNSPECIFIED.);
#297=B_SPLINE_CURVE_WITH_KNOTS('',3,(#7858,#7859,#7860,#7861,#7862,#7863,
#7864,#7865,#7866,#7867,#7868,#7869,#7870),.UNSPECIFIED.,.F.,.F.,(4,3,3,
3,4),(0.,0.0716322252392673,0.143264450478534,0.238774084130891,0.334283717783247),
 .UNSPECIFIED.);
#298=B_SPLINE_CURVE_WITH_KNOTS('',3,(#7871,#7872,#7873,#7874),
 .UNSPECIFIED.,.F.,.F.,(4,4),(-1.64459338547828E-15,2.09998933244218),
 .UNSPECIFIED.);
#299=B_SPLINE_CURVE_WITH_KNOTS('',3,(#7875,#7876,#7877,#7878),
 .UNSPECIFIED.,.F.,.F.,(4,4),(-2.09998933244218,1.64459338547828E-15),
 .UNSPECIFIED.);
#300=B_SPLINE_SURFACE_WITH_KNOTS('',3,3,((#5724,#5725,#5726,#5727),(#5728,
#5729,#5730,#5731),(#5732,#5733,#5734,#5735),(#5736,#5737,#5738,#5739),
(#5740,#5741,#5742,#5743)),.UNSPECIFIED.,.F.,.F.,.F.,(4,1,4),(4,4),(0.,
0.571428571428571,1.),(0.,0.314873215025081),.UNSPECIFIED.);
#301=B_SPLINE_SURFACE_WITH_KNOTS('',3,3,((#5763,#5764,#5765,#5766),(#5767,
#5768,#5769,#5770),(#5771,#5772,#5773,#5774),(#5775,#5776,#5777,#5778),
(#5779,#5780,#5781,#5782)),.UNSPECIFIED.,.F.,.F.,.F.,(4,1,4),(4,4),(0.,
0.571428571428571,1.),(0.,0.0585005125063144),.UNSPECIFIED.);
#302=B_SPLINE_SURFACE_WITH_KNOTS('',3,3,((#5794,#5795,#5796,#5797,#5798,
#5799,#5800),(#5801,#5802,#5803,#5804,#5805,#5806,#5807),(#5808,#5809,#5810,
#5811,#5812,#5813,#5814),(#5815,#5816,#5817,#5818,#5819,#5820,#5821),(#5822,
#5823,#5824,#5825,#5826,#5827,#5828)),.UNSPECIFIED.,.F.,.F.,.F.,(4,1,4),
(4,1,1,1,4),(0.,0.571428571428571,1.),(0.0969258860400105,0.307478806147851,
0.728584646363533,1.14969048657921,1.5707963267949),.UNSPECIFIED.);
#303=B_SPLINE_SURFACE_WITH_KNOTS('',3,3,((#5909,#5910,#5911,#5912),(#5913,
#5914,#5915,#5916),(#5917,#5918,#5919,#5920),(#5921,#5922,#5923,#5924),
(#5925,#5926,#5927,#5928)),.UNSPECIFIED.,.F.,.F.,.F.,(4,1,4),(4,4),(0.,
0.571428571428571,1.),(0.,0.31487081906698),.UNSPECIFIED.);
#304=B_SPLINE_SURFACE_WITH_KNOTS('',3,3,((#5948,#5949,#5950,#5951),(#5952,
#5953,#5954,#5955),(#5956,#5957,#5958,#5959),(#5960,#5961,#5962,#5963),
(#5964,#5965,#5966,#5967)),.UNSPECIFIED.,.F.,.F.,.F.,(4,1,4),(4,4),(0.,
0.571428571428571,1.),(0.,0.0585005125063158),.UNSPECIFIED.);
#305=B_SPLINE_SURFACE_WITH_KNOTS('',3,3,((#5979,#5980,#5981,#5982,#5983,
#5984),(#5985,#5986,#5987,#5988,#5989,#5990),(#5991,#5992,#5993,#5994,#5995,
#5996),(#5997,#5998,#5999,#6000,#6001,#6002),(#6003,#6004,#6005,#6006,#6007,
#6008)),.UNSPECIFIED.,.F.,.F.,.F.,(4,1,4),(4,1,1,4),(0.,0.571428571428571,
1.),(-1.5707963267949,-0.939137566471373,-0.518031726255691,-0.0969258860400086),
 .UNSPECIFIED.);
#306=B_SPLINE_SURFACE_WITH_KNOTS('',3,3,((#6022,#6023,#6024,#6025,#6026,
#6027),(#6028,#6029,#6030,#6031,#6032,#6033),(#6034,#6035,#6036,#6037,#6038,
#6039),(#6040,#6041,#6042,#6043,#6044,#6045),(#6046,#6047,#6048,#6049,#6050,
#6051)),.UNSPECIFIED.,.F.,.F.,.F.,(4,1,4),(4,1,1,4),(0.,0.571428571428571,
1.),(-1.5707963267949,-0.939137566471373,-0.51803172625569,-0.0969258860400074),
 .UNSPECIFIED.);
#307=B_SPLINE_SURFACE_WITH_KNOTS('',3,3,((#6057,#6058,#6059,#6060),(#6061,
#6062,#6063,#6064),(#6065,#6066,#6067,#6068),(#6069,#6070,#6071,#6072),
(#6073,#6074,#6075,#6076)),.UNSPECIFIED.,.F.,.F.,.F.,(4,1,4),(4,4),(0.,
0.571428571428571,1.),(0.,0.0585005125063147),.UNSPECIFIED.);
#308=B_SPLINE_SURFACE_WITH_KNOTS('',3,3,((#6094,#6095,#6096,#6097,#6098),
(#6099,#6100,#6101,#6102,#6103),(#6104,#6105,#6106,#6107,#6108),(#6109,
#6110,#6111,#6112,#6113),(#6114,#6115,#6116,#6117,#6118)),.UNSPECIFIED.,
 .F.,.F.,.F.,(4,1,4),(4,1,4),(0.,0.571428571428571,1.),(0.792810545672275,
0.988925248429188,1.25041151877174),.UNSPECIFIED.);
#309=B_SPLINE_SURFACE_WITH_KNOTS('',3,3,((#6174,#6175,#6176,#6177,#6178),
(#6179,#6180,#6181,#6182,#6183),(#6184,#6185,#6186,#6187,#6188),(#6189,
#6190,#6191,#6192,#6193),(#6194,#6195,#6196,#6197,#6198)),.UNSPECIFIED.,
 .F.,.F.,.F.,(4,1,4),(4,1,4),(0.,0.571428571428571,1.),(-1.5707963267949,
-0.999178609866638,-0.237021653962293),.UNSPECIFIED.);
#310=B_SPLINE_SURFACE_WITH_KNOTS('',3,3,((#6212,#6213,#6214,#6215),(#6216,
#6217,#6218,#6219),(#6220,#6221,#6222,#6223),(#6224,#6225,#6226,#6227),
(#6228,#6229,#6230,#6231)),.UNSPECIFIED.,.F.,.F.,.F.,(4,1,4),(4,4),(0.,
0.571428571428571,1.),(0.,0.0585005125063158),.UNSPECIFIED.);
#311=B_SPLINE_SURFACE_WITH_KNOTS('',3,3,((#6243,#6244,#6245,#6246,#6247,
#6248,#6249),(#6250,#6251,#6252,#6253,#6254,#6255,#6256),(#6257,#6258,#6259,
#6260,#6261,#6262,#6263),(#6264,#6265,#6266,#6267,#6268,#6269,#6270),(#6271,
#6272,#6273,#6274,#6275,#6276,#6277)),.UNSPECIFIED.,.F.,.F.,.F.,(4,1,4),
(4,1,1,1,4),(0.,0.571428571428571,1.),(0.0969258860400078,0.307478806147849,
0.728584646363532,1.14969048657921,1.5707963267949),.UNSPECIFIED.);
#312=B_SPLINE_SURFACE_WITH_KNOTS('',3,3,((#6281,#6282,#6283,#6284),(#6285,
#6286,#6287,#6288),(#6289,#6290,#6291,#6292),(#6293,#6294,#6295,#6296),
(#6297,#6298,#6299,#6300)),.UNSPECIFIED.,.F.,.F.,.F.,(4,1,4),(4,4),(0.,
0.571428571428571,1.),(0.793286355786688,1.25278641295821),
 .UNSPECIFIED.);
#313=B_SPLINE_SURFACE_WITH_KNOTS('',3,3,((#6358,#6359,#6360,#6361,#6362),
(#6363,#6364,#6365,#6366,#6367),(#6368,#6369,#6370,#6371,#6372),(#6373,
#6374,#6375,#6376,#6377),(#6378,#6379,#6380,#6381,#6382)),.UNSPECIFIED.,
 .F.,.F.,.F.,(4,1,4),(4,1,4),(0.,0.571428571428571,1.),(-1.5707963267949,
-0.99917860986662,-0.23702165396225),.UNSPECIFIED.);
#314=B_SPLINE_SURFACE_WITH_KNOTS('',3,3,((#6425,#6426,#6427,#6428),(#6429,
#6430,#6431,#6432),(#6433,#6434,#6435,#6436),(#6437,#6438,#6439,#6440),
(#6441,#6442,#6443,#6444)),.UNSPECIFIED.,.F.,.F.,.F.,(4,1,4),(4,4),(0.,
0.571428571428571,1.),(0.98361909310298,1.35639146206056),.UNSPECIFIED.);
#315=B_SPLINE_SURFACE_WITH_KNOTS('',3,3,((#6458,#6459,#6460,#6461,#6462,
#6463,#6464,#6465,#6466,#6467),(#6468,#6469,#6470,#6471,#6472,#6473,#6474,
#6475,#6476,#6477),(#6478,#6479,#6480,#6481,#6482,#6483,#6484,#6485,#6486,
#6487),(#6488,#6489,#6490,#6491,#6492,#6493,#6494,#6495,#6496,#6497),(#6498,
#6499,#6500,#6501,#6502,#6503,#6504,#6505,#6506,#6507)),.UNSPECIFIED.,.F.,
 .F.,.F.,(4,1,4),(4,1,1,1,1,1,1,4),(0.,0.571428571428571,1.),(-1.35639146206079,
-0.968851044329184,-0.581310626597581,-0.193770208865978,0.193770208865625,
0.581310626597229,0.968851044328832,1.35639146206044),.UNSPECIFIED.);
#316=B_SPLINE_SURFACE_WITH_KNOTS('',3,3,((#6513,#6514,#6515,#6516),(#6517,
#6518,#6519,#6520),(#6521,#6522,#6523,#6524),(#6525,#6526,#6527,#6528),
(#6529,#6530,#6531,#6532)),.UNSPECIFIED.,.F.,.F.,.F.,(4,1,4),(4,4),(0.,
0.571428571428571,1.),(4.92679384511897,5.29956633635466),.UNSPECIFIED.);
#317=B_SPLINE_SURFACE_WITH_KNOTS('',3,3,((#6727,#6728,#6729,#6730,#6731),
(#6732,#6733,#6734,#6735,#6736),(#6737,#6738,#6739,#6740,#6741),(#6742,
#6743,#6744,#6745,#6746),(#6747,#6748,#6749,#6750,#6751),(#6752,#6753,#6754,
#6755,#6756),(#6757,#6758,#6759,#6760,#6761)),.UNSPECIFIED.,.F.,.F.,.F.,
(4,1,1,1,4),(4,1,4),(0.,0.285714285714286,0.571428571428571,0.785714285714286,
1.),(2.84420950871177E-11,0.45774596523445,0.801055439138956),
 .UNSPECIFIED.);
#318=B_SPLINE_SURFACE_WITH_KNOTS('',3,3,((#6806,#6807,#6808,#6809),(#6810,
#6811,#6812,#6813),(#6814,#6815,#6816,#6817),(#6818,#6819,#6820,#6821),
(#6822,#6823,#6824,#6825),(#6826,#6827,#6828,#6829),(#6830,#6831,#6832,
#6833)),.UNSPECIFIED.,.F.,.F.,.F.,(4,1,1,1,4),(4,4),(0.,0.285714285714286,
0.571428571428571,0.785714285714286,1.),(0.801055439138956,2.06290888015454),
 .UNSPECIFIED.);
#319=B_SPLINE_SURFACE_WITH_KNOTS('',3,3,((#6851,#6852,#6853,#6854,#6855),
(#6856,#6857,#6858,#6859,#6860),(#6861,#6862,#6863,#6864,#6865),(#6866,
#6867,#6868,#6869,#6870),(#6871,#6872,#6873,#6874,#6875),(#6876,#6877,#6878,
#6879,#6880),(#6881,#6882,#6883,#6884,#6885)),.UNSPECIFIED.,.F.,.F.,.F.,
(4,1,1,1,4),(4,1,4),(0.,0.285714285714286,0.571428571428571,0.785714285714286,
1.),(2.06290887470076,2.069883451706,2.07918288771298),.UNSPECIFIED.);
#320=B_SPLINE_SURFACE_WITH_KNOTS('',3,3,((#6905,#6906,#6907,#6908),(#6909,
#6910,#6911,#6912),(#6913,#6914,#6915,#6916),(#6917,#6918,#6919,#6920),
(#6921,#6922,#6923,#6924),(#6925,#6926,#6927,#6928),(#6929,#6930,#6931,
#6932)),.UNSPECIFIED.,.F.,.F.,.F.,(4,1,1,1,4),(4,4),(0.,0.285714285714286,
0.571428571428571,0.785714285714286,1.),(2.07918288771299,2.19760564616015),
 .UNSPECIFIED.);
#321=B_SPLINE_SURFACE_WITH_KNOTS('',3,3,((#6950,#6951,#6952,#6953,#6954,
#6955,#6956,#6957,#6958,#6959,#6960,#6961),(#6962,#6963,#6964,#6965,#6966,
#6967,#6968,#6969,#6970,#6971,#6972,#6973),(#6974,#6975,#6976,#6977,#6978,
#6979,#6980,#6981,#6982,#6983,#6984,#6985),(#6986,#6987,#6988,#6989,#6990,
#6991,#6992,#6993,#6994,#6995,#6996,#6997),(#6998,#6999,#7000,#7001,#7002,
#7003,#7004,#7005,#7006,#7007,#7008,#7009),(#7010,#7011,#7012,#7013,#7014,
#7015,#7016,#7017,#7018,#7019,#7020,#7021),(#7022,#7023,#7024,#7025,#7026,
#7027,#7028,#7029,#7030,#7031,#7032,#7033)),.UNSPECIFIED.,.F.,.F.,.F.,(4,
1,1,1,4),(4,1,1,1,1,1,1,1,1,4),(0.,0.285714285714286,0.571428571428571,
0.785714285714286,1.),(2.19760564621546,2.99612878215101,3.79465191808657,
4.32700067537694,4.59317505402212,4.85934943266731,5.39169818995768,6.19022132589323,
6.98874446182879,7.78726759776434),.UNSPECIFIED.);
#322=B_SPLINE_SURFACE_WITH_KNOTS('',3,3,((#7067,#7068,#7069,#7070),(#7071,
#7072,#7073,#7074),(#7075,#7076,#7077,#7078),(#7079,#7080,#7081,#7082),
(#7083,#7084,#7085,#7086),(#7087,#7088,#7089,#7090),(#7091,#7092,#7093,
#7094)),.UNSPECIFIED.,.F.,.F.,.F.,(4,1,1,1,4),(4,4),(0.,0.285714285714286,
0.571428571428571,0.785714285714286,1.),(7.78726759776434,7.9056903551329),
 .UNSPECIFIED.);
#323=B_SPLINE_SURFACE_WITH_KNOTS('',3,3,((#7112,#7113,#7114,#7115,#7116),
(#7117,#7118,#7119,#7120,#7121),(#7122,#7123,#7124,#7125,#7126),(#7127,
#7128,#7129,#7130,#7131),(#7132,#7133,#7134,#7135,#7136),(#7137,#7138,#7139,
#7140,#7141),(#7142,#7143,#7144,#7145,#7146)),.UNSPECIFIED.,.F.,.F.,.F.,
(4,1,1,1,4),(4,1,4),(0.,0.285714285714286,0.571428571428571,0.785714285714286,
1.),(7.90569035513291,7.91266493450595,7.92196437367001),.UNSPECIFIED.);
#324=B_SPLINE_SURFACE_WITH_KNOTS('',3,3,((#7166,#7167,#7168,#7169),(#7170,
#7171,#7172,#7173),(#7174,#7175,#7176,#7177),(#7178,#7179,#7180,#7181),
(#7182,#7183,#7184,#7185),(#7186,#7187,#7188,#7189),(#7190,#7191,#7192,
#7193)),.UNSPECIFIED.,.F.,.F.,.F.,(4,1,1,1,4),(4,4),(0.,0.285714285714286,
0.571428571428571,0.785714285714286,1.),(7.92196436821623,9.18381780243075),
 .UNSPECIFIED.);
#325=B_SPLINE_SURFACE_WITH_KNOTS('',3,3,((#7211,#7212,#7213,#7214),(#7215,
#7216,#7217,#7218),(#7219,#7220,#7221,#7222),(#7223,#7224,#7225,#7226),
(#7227,#7228,#7229,#7230),(#7231,#7232,#7233,#7234),(#7235,#7236,#7237,
#7238)),.UNSPECIFIED.,.F.,.F.,.F.,(4,1,1,1,4),(4,4),(0.,0.285714285714286,
0.571428571428571,0.785714285714286,1.),(9.18381780243075,9.50411765280707),
 .UNSPECIFIED.);
#326=B_SPLINE_SURFACE_WITH_KNOTS('',3,3,((#7256,#7257,#7258,#7259,#7260),
(#7261,#7262,#7263,#7264,#7265),(#7266,#7267,#7268,#7269,#7270),(#7271,
#7272,#7273,#7274,#7275),(#7276,#7277,#7278,#7279,#7280),(#7281,#7282,#7283,
#7284,#7285),(#7286,#7287,#7288,#7289,#7290)),.UNSPECIFIED.,.F.,.F.,.F.,
(4,1,1,1,4),(4,1,4),(0.,0.285714285714286,0.571428571428571,0.785714285714286,
1.),(9.50411765345197,9.71136698388339,9.98769942445863),.UNSPECIFIED.);
#327=B_SPLINE_SURFACE_WITH_KNOTS('',3,3,((#7320,#7321,#7322,#7323),(#7324,
#7325,#7326,#7327),(#7328,#7329,#7330,#7331),(#7332,#7333,#7334,#7335)),
 .UNSPECIFIED.,.F.,.F.,.F.,(4,4),(4,4),(0.,0.00685219205909856),(9.98769942445863,
11.987699095758),.UNSPECIFIED.);
#328=B_SPLINE_SURFACE_WITH_KNOTS('',3,3,((#7363,#7364,#7365,#7366),(#7367,
#7368,#7369,#7370),(#7371,#7372,#7373,#7374),(#7375,#7376,#7377,#7378),
(#7379,#7380,#7381,#7382),(#7383,#7384,#7385,#7386),(#7387,#7388,#7389,
#7390)),.UNSPECIFIED.,.F.,.F.,.F.,(4,1,1,1,4),(4,4),(0.,0.285714285714286,
0.571428571428571,0.785714285714286,1.),(10.3397956275468,12.4397849599923),
 .UNSPECIFIED.);
#329=B_SPLINE_SURFACE_WITH_KNOTS('',3,3,((#7423,#7424,#7425,#7426,#7427),
(#7428,#7429,#7430,#7431,#7432),(#7433,#7434,#7435,#7436,#7437),(#7438,
#7439,#7440,#7441,#7442),(#7443,#7444,#7445,#7446,#7447),(#7448,#7449,#7450,
#7451,#7452),(#7453,#7454,#7455,#7456,#7457)),.UNSPECIFIED.,.F.,.F.,.F.,
(4,1,1,1,4),(4,1,4),(0.,0.285714285714286,0.571428571428571,0.785714285714286,
1.),(-10.3397956275468,-10.2806762057263,-10.2018503099656),
 .UNSPECIFIED.);
#330=B_SPLINE_SURFACE_WITH_KNOTS('',3,3,((#7477,#7478,#7479,#7480),(#7481,
#7482,#7483,#7484),(#7485,#7486,#7487,#7488),(#7489,#7490,#7491,#7492),
(#7493,#7494,#7495,#7496),(#7497,#7498,#7499,#7500),(#7501,#7502,#7503,
#7504)),.UNSPECIFIED.,.F.,.F.,.F.,(4,1,1,1,4),(4,4),(0.,0.285714285714286,
0.571428571428571,0.785714285714286,1.),(8.93986452633385,10.2018503099635),
 .UNSPECIFIED.);
#331=B_SPLINE_SURFACE_WITH_KNOTS('',3,3,((#7522,#7523,#7524,#7525,#7526),
(#7527,#7528,#7529,#7530,#7531),(#7532,#7533,#7534,#7535,#7536),(#7537,
#7538,#7539,#7540,#7541),(#7542,#7543,#7544,#7545,#7546),(#7547,#7548,#7549,
#7550,#7551),(#7552,#7553,#7554,#7555,#7556)),.UNSPECIFIED.,.F.,.F.,.F.,
(4,1,1,1,4),(4,1,4),(0.,0.285714285714286,0.571428571428571,0.785714285714286,
1.),(8.33860637357674,8.68218245774598,8.93986452087291),.UNSPECIFIED.);
#332=B_SPLINE_SURFACE_WITH_KNOTS('',3,3,((#7576,#7577,#7578,#7579,#7580,
#7581,#7582,#7583,#7584,#7585),(#7586,#7587,#7588,#7589,#7590,#7591,#7592,
#7593,#7594,#7595),(#7596,#7597,#7598,#7599,#7600,#7601,#7602,#7603,#7604,
#7605),(#7606,#7607,#7608,#7609,#7610,#7611,#7612,#7613,#7614,#7615),(#7616,
#7617,#7618,#7619,#7620,#7621,#7622,#7623,#7624,#7625),(#7626,#7627,#7628,
#7629,#7630,#7631,#7632,#7633,#7634,#7635),(#7636,#7637,#7638,#7639,#7640,
#7641,#7642,#7643,#7644,#7645)),.UNSPECIFIED.,.F.,.F.,.F.,(4,1,1,1,4),(4,
1,1,1,1,1,1,4),(0.,0.285714285714286,0.571428571428571,0.785714285714286,
1.),(-8.33860637357674,-7.73325954416072,-7.12791271474469,-6.52256588532867,
-5.91721905591265,-5.31187222649662,-4.7065253970806,-4.10117856766458),
 .UNSPECIFIED.);
#333=B_SPLINE_SURFACE_WITH_KNOTS('',3,3,((#7675,#7676,#7677,#7678,#7679),
(#7680,#7681,#7682,#7683,#7684),(#7685,#7686,#7687,#7688,#7689),(#7690,
#7691,#7692,#7693,#7694),(#7695,#7696,#7697,#7698,#7699),(#7700,#7701,#7702,
#7703,#7704),(#7705,#7706,#7707,#7708,#7709)),.UNSPECIFIED.,.F.,.F.,.F.,
(4,1,1,1,4),(4,1,4),(0.,0.285714285714286,0.571428571428571,0.785714285714286,
1.),(3.4999204445805,3.75760250536717,4.10117858641605),.UNSPECIFIED.);
#334=B_SPLINE_SURFACE_WITH_KNOTS('',3,3,((#7729,#7730,#7731,#7732),(#7733,
#7734,#7735,#7736),(#7737,#7738,#7739,#7740),(#7741,#7742,#7743,#7744),
(#7745,#7746,#7747,#7748),(#7749,#7750,#7751,#7752),(#7753,#7754,#7755,
#7756)),.UNSPECIFIED.,.F.,.F.,.F.,(4,1,1,1,4),(4,4),(0.,0.285714285714286,
0.571428571428571,0.785714285714286,1.),(-3.49992043911957,-2.23793465002183),
 .UNSPECIFIED.);
#335=B_SPLINE_SURFACE_WITH_KNOTS('',3,3,((#7774,#7775,#7776,#7777,#7778),
(#7779,#7780,#7781,#7782,#7783),(#7784,#7785,#7786,#7787,#7788),(#7789,
#7790,#7791,#7792,#7793),(#7794,#7795,#7796,#7797,#7798),(#7799,#7800,#7801,
#7802,#7803),(#7804,#7805,#7806,#7807,#7808)),.UNSPECIFIED.,.F.,.F.,.F.,
(4,1,1,1,4),(4,1,4),(0.,0.285714285714286,0.571428571428571,0.785714285714286,
1.),(-2.23793465002292,-2.17881522820334,-2.09998933244391),
 .UNSPECIFIED.);
#336=B_SPLINE_SURFACE_WITH_KNOTS('',3,3,((#7828,#7829,#7830,#7831),(#7832,
#7833,#7834,#7835),(#7836,#7837,#7838,#7839),(#7840,#7841,#7842,#7843),
(#7844,#7845,#7846,#7847),(#7848,#7849,#7850,#7851),(#7852,#7853,#7854,
#7855)),.UNSPECIFIED.,.F.,.F.,.F.,(4,1,1,1,4),(4,4),(0.,0.285714285714286,
0.571428571428571,0.785714285714286,1.),(-2.09998933244218,1.64459338547828E-15),
 .UNSPECIFIED.);
#337=FACE_BOUND('',#770,.T.);
#338=FACE_BOUND('',#771,.T.);
#339=FACE_BOUND('',#775,.T.);
#340=FACE_BOUND('',#776,.T.);
#341=FACE_BOUND('',#786,.T.);
#342=FACE_BOUND('',#797,.T.);
#343=FACE_BOUND('',#816,.T.);
#344=FACE_BOUND('',#839,.T.);
#345=FACE_BOUND('',#845,.T.);
#346=FACE_BOUND('',#861,.T.);
#347=FACE_BOUND('',#862,.T.);
#348=FACE_BOUND('',#905,.T.);
#349=FACE_BOUND('',#906,.T.);
#350=FACE_BOUND('',#927,.T.);
#351=FACE_BOUND('',#928,.T.);
#352=FACE_BOUND('',#931,.T.);
#353=FACE_BOUND('',#935,.T.);
#354=FACE_BOUND('',#939,.T.);
#355=FACE_BOUND('',#940,.T.);
#356=FACE_BOUND('',#946,.T.);
#357=FACE_BOUND('',#947,.T.);
#358=FACE_BOUND('',#951,.T.);
#359=FACE_BOUND('',#962,.T.);
#360=FACE_BOUND('',#975,.T.);
#361=FACE_BOUND('',#984,.T.);
#362=FACE_BOUND('',#986,.T.);
#363=FACE_BOUND('',#996,.T.);
#364=FACE_BOUND('',#1003,.T.);
#365=FACE_BOUND('',#1006,.T.);
#366=FACE_BOUND('',#1012,.T.);
#367=FACE_BOUND('',#1015,.T.);
#368=FACE_BOUND('',#1017,.T.);
#369=CIRCLE('',#4122,3.);
#370=CIRCLE('',#4123,3.);
#371=CIRCLE('',#4126,6.);
#372=CIRCLE('',#4127,6.);
#373=CIRCLE('',#4129,28.);
#374=CIRCLE('',#4130,3.);
#375=CIRCLE('',#4131,3.);
#376=CIRCLE('',#4132,28.);
#377=CIRCLE('',#4133,4.);
#378=CIRCLE('',#4134,3.99999999999999);
#379=CIRCLE('',#4135,3.);
#380=CIRCLE('',#4136,3.);
#381=CIRCLE('',#4138,3.);
#382=CIRCLE('',#4139,28.);
#383=CIRCLE('',#4140,25.);
#384=CIRCLE('',#4141,3.);
#385=CIRCLE('',#4145,32.);
#386=CIRCLE('',#4146,3.);
#387=CIRCLE('',#4147,35.);
#388=CIRCLE('',#4149,3.);
#389=CIRCLE('',#4151,3.);
#390=CIRCLE('',#4153,3.);
#391=CIRCLE('',#4155,4.);
#392=CIRCLE('',#4159,35.);
#393=CIRCLE('',#4160,3.);
#394=CIRCLE('',#4161,32.);
#395=CIRCLE('',#4163,3.);
#396=CIRCLE('',#4164,3.);
#397=CIRCLE('',#4165,3.);
#398=CIRCLE('',#4167,3.00000000000001);
#399=CIRCLE('',#4168,25.);
#400=CIRCLE('',#4169,28.);
#401=CIRCLE('',#4170,3.);
#402=CIRCLE('',#4174,3.);
#403=CIRCLE('',#4176,4.);
#404=CIRCLE('',#4179,3.);
#405=CIRCLE('',#4182,3.);
#406=CIRCLE('',#4184,3.);
#407=CIRCLE('',#4185,28.);
#408=CIRCLE('',#4186,25.);
#409=CIRCLE('',#4188,28.);
#410=CIRCLE('',#4192,3.00000000000002);
#411=CIRCLE('',#4195,3.);
#412=CIRCLE('',#4196,28.);
#413=CIRCLE('',#4197,2.99999999999997);
#414=CIRCLE('',#4198,25.);
#415=CIRCLE('',#4199,3.);
#416=CIRCLE('',#4207,3.99999999999999);
#417=CIRCLE('',#4209,3.);
#418=CIRCLE('',#4211,3.00000000000002);
#419=CIRCLE('',#4213,8.99999999999999);
#420=CIRCLE('',#4214,3.00000000000002);
#421=CIRCLE('',#4215,5.99999999999999);
#422=CIRCLE('',#4217,3.00000000000005);
#423=CIRCLE('',#4219,3.);
#424=CIRCLE('',#4221,3.);
#425=CIRCLE('',#4227,5.99999999999999);
#426=CIRCLE('',#4228,3.);
#427=CIRCLE('',#4229,8.99999999999999);
#428=CIRCLE('',#4231,3.);
#429=CIRCLE('',#4233,3.);
#430=CIRCLE('',#4235,3.);
#431=CIRCLE('',#4237,3.);
#432=CIRCLE('',#4253,9.5);
#433=CIRCLE('',#4256,9.5);
#434=CIRCLE('',#4259,3.);
#435=CIRCLE('',#4262,3.99999999999999);
#436=CIRCLE('',#4265,4.);
#437=CIRCLE('',#4267,28.);
#438=CIRCLE('',#4270,3.99999999999999);
#439=CIRCLE('',#4274,3.);
#440=CIRCLE('',#4277,3.);
#441=CIRCLE('',#4286,3.);
#442=CIRCLE('',#4287,3.);
#443=CIRCLE('',#4290,3.);
#444=CIRCLE('',#4291,3.);
#445=CIRCLE('',#4295,17.5000000000459);
#446=CIRCLE('',#4296,17.5);
#447=CIRCLE('',#4299,3.00000000000001);
#448=CIRCLE('',#4307,2.99999999999999);
#449=CIRCLE('',#4309,3.00000000000001);
#450=CIRCLE('',#4316,3.00000000000001);
#451=CIRCLE('',#4317,3.00000000000001);
#452=CIRCLE('',#4320,2.99999999999998);
#453=CIRCLE('',#4321,2.99999999999998);
#454=CIRCLE('',#4328,1.);
#455=CIRCLE('',#4330,1.);
#456=CIRCLE('',#4332,9.5);
#457=CIRCLE('',#4333,9.5);
#458=CIRCLE('',#4346,5.25);
#459=CIRCLE('',#4347,3.25);
#460=CIRCLE('',#4349,5.25);
#461=CIRCLE('',#4351,3.25);
#462=CIRCLE('',#4353,5.25);
#463=CIRCLE('',#4354,3.25);
#464=CIRCLE('',#4356,5.25);
#465=CIRCLE('',#4358,3.25);
#466=CIRCLE('',#4367,3.);
#467=CIRCLE('',#4368,1.);
#468=CIRCLE('',#4369,4.);
#469=CIRCLE('',#4370,3.);
#470=CIRCLE('',#4372,3.);
#471=CIRCLE('',#4374,5.);
#472=CIRCLE('',#4383,4.);
#473=CIRCLE('',#4384,1.);
#474=CIRCLE('',#4385,5.);
#475=CIRCLE('',#4386,5.);
#476=CIRCLE('',#4392,6.5);
#477=CIRCLE('',#4393,9.5);
#478=CIRCLE('',#4399,6.5);
#479=CIRCLE('',#4400,9.5);
#480=CIRCLE('',#4402,6.5);
#481=CIRCLE('',#4403,6.5);
#482=CIRCLE('',#4404,9.5);
#483=CIRCLE('',#4405,9.5);
#484=CIRCLE('',#4407,9.5);
#485=CIRCLE('',#4408,6.5);
#486=CIRCLE('',#4410,9.5);
#487=CIRCLE('',#4412,6.5);
#488=CIRCLE('',#4416,1.25);
#489=CIRCLE('',#4417,1.25);
#490=CIRCLE('',#4419,5.00000007450581);
#491=CIRCLE('',#4420,5.00000007450581);
#492=CIRCLE('',#4423,0.999999999999998);
#493=CIRCLE('',#4424,0.999999999999998);
#494=CIRCLE('',#4426,15.);
#495=CIRCLE('',#4427,15.);
#496=CIRCLE('',#4429,1.);
#497=CIRCLE('',#4430,1.);
#498=CIRCLE('',#4438,1.9);
#499=CIRCLE('',#4439,1.9);
#500=CIRCLE('',#4441,1.9);
#501=CIRCLE('',#4442,1.9);
#502=CIRCLE('',#4444,1.9);
#503=CIRCLE('',#4446,1.);
#504=CIRCLE('',#4447,1.);
#505=CIRCLE('',#4450,1.9);
#506=CIRCLE('',#4454,8.);
#507=CIRCLE('',#4455,1.5);
#508=CIRCLE('',#4456,9.5);
#509=CIRCLE('',#4457,9.5);
#510=CIRCLE('',#4459,9.5);
#511=CIRCLE('',#4460,9.5);
#512=CIRCLE('',#4463,9.5);
#513=CIRCLE('',#4464,9.5);
#514=CIRCLE('',#4465,4.1);
#515=CIRCLE('',#4467,9.5);
#516=CIRCLE('',#4469,6.5);
#517=CIRCLE('',#4471,6.5);
#518=CIRCLE('',#4473,6.50000009685755);
#519=CIRCLE('',#4474,4.75);
#520=CIRCLE('',#4476,6.50000009685755);
#521=CIRCLE('',#4479,4.75);
#522=CIRCLE('',#4481,6.5);
#523=CIRCLE('',#4482,6.5);
#524=CIRCLE('',#4485,8.);
#525=CIRCLE('',#4486,8.);
#526=FACE_OUTER_BOUND('',#761,.T.);
#527=FACE_OUTER_BOUND('',#762,.T.);
#528=FACE_OUTER_BOUND('',#763,.T.);
#529=FACE_OUTER_BOUND('',#764,.T.);
#530=FACE_OUTER_BOUND('',#765,.T.);
#531=FACE_OUTER_BOUND('',#766,.T.);
#532=FACE_OUTER_BOUND('',#767,.T.);
#533=FACE_OUTER_BOUND('',#768,.T.);
#534=FACE_OUTER_BOUND('',#769,.T.);
#535=FACE_OUTER_BOUND('',#772,.T.);
#536=FACE_OUTER_BOUND('',#773,.T.);
#537=FACE_OUTER_BOUND('',#774,.T.);
#538=FACE_OUTER_BOUND('',#777,.T.);
#539=FACE_OUTER_BOUND('',#778,.T.);
#540=FACE_OUTER_BOUND('',#779,.T.);
#541=FACE_OUTER_BOUND('',#780,.T.);
#542=FACE_OUTER_BOUND('',#781,.T.);
#543=FACE_OUTER_BOUND('',#782,.T.);
#544=FACE_OUTER_BOUND('',#783,.T.);
#545=FACE_OUTER_BOUND('',#784,.T.);
#546=FACE_OUTER_BOUND('',#785,.T.);
#547=FACE_OUTER_BOUND('',#787,.T.);
#548=FACE_OUTER_BOUND('',#788,.T.);
#549=FACE_OUTER_BOUND('',#789,.T.);
#550=FACE_OUTER_BOUND('',#790,.T.);
#551=FACE_OUTER_BOUND('',#791,.T.);
#552=FACE_OUTER_BOUND('',#792,.T.);
#553=FACE_OUTER_BOUND('',#793,.T.);
#554=FACE_OUTER_BOUND('',#794,.T.);
#555=FACE_OUTER_BOUND('',#795,.T.);
#556=FACE_OUTER_BOUND('',#796,.T.);
#557=FACE_OUTER_BOUND('',#798,.T.);
#558=FACE_OUTER_BOUND('',#799,.T.);
#559=FACE_OUTER_BOUND('',#800,.T.);
#560=FACE_OUTER_BOUND('',#801,.T.);
#561=FACE_OUTER_BOUND('',#802,.T.);
#562=FACE_OUTER_BOUND('',#803,.T.);
#563=FACE_OUTER_BOUND('',#804,.T.);
#564=FACE_OUTER_BOUND('',#805,.T.);
#565=FACE_OUTER_BOUND('',#806,.T.);
#566=FACE_OUTER_BOUND('',#807,.T.);
#567=FACE_OUTER_BOUND('',#808,.T.);
#568=FACE_OUTER_BOUND('',#809,.T.);
#569=FACE_OUTER_BOUND('',#810,.T.);
#570=FACE_OUTER_BOUND('',#811,.T.);
#571=FACE_OUTER_BOUND('',#812,.T.);
#572=FACE_OUTER_BOUND('',#813,.T.);
#573=FACE_OUTER_BOUND('',#814,.T.);
#574=FACE_OUTER_BOUND('',#815,.T.);
#575=FACE_OUTER_BOUND('',#817,.T.);
#576=FACE_OUTER_BOUND('',#818,.T.);
#577=FACE_OUTER_BOUND('',#819,.T.);
#578=FACE_OUTER_BOUND('',#820,.T.);
#579=FACE_OUTER_BOUND('',#821,.T.);
#580=FACE_OUTER_BOUND('',#822,.T.);
#581=FACE_OUTER_BOUND('',#823,.T.);
#582=FACE_OUTER_BOUND('',#824,.T.);
#583=FACE_OUTER_BOUND('',#825,.T.);
#584=FACE_OUTER_BOUND('',#826,.T.);
#585=FACE_OUTER_BOUND('',#827,.T.);
#586=FACE_OUTER_BOUND('',#828,.T.);
#587=FACE_OUTER_BOUND('',#829,.T.);
#588=FACE_OUTER_BOUND('',#830,.T.);
#589=FACE_OUTER_BOUND('',#831,.T.);
#590=FACE_OUTER_BOUND('',#832,.T.);
#591=FACE_OUTER_BOUND('',#833,.T.);
#592=FACE_OUTER_BOUND('',#834,.T.);
#593=FACE_OUTER_BOUND('',#835,.T.);
#594=FACE_OUTER_BOUND('',#836,.T.);
#595=FACE_OUTER_BOUND('',#837,.T.);
#596=FACE_OUTER_BOUND('',#838,.T.);
#597=FACE_OUTER_BOUND('',#840,.T.);
#598=FACE_OUTER_BOUND('',#841,.T.);
#599=FACE_OUTER_BOUND('',#842,.T.);
#600=FACE_OUTER_BOUND('',#843,.T.);
#601=FACE_OUTER_BOUND('',#844,.T.);
#602=FACE_OUTER_BOUND('',#846,.T.);
#603=FACE_OUTER_BOUND('',#847,.T.);
#604=FACE_OUTER_BOUND('',#848,.T.);
#605=FACE_OUTER_BOUND('',#849,.T.);
#606=FACE_OUTER_BOUND('',#850,.T.);
#607=FACE_OUTER_BOUND('',#851,.T.);
#608=FACE_OUTER_BOUND('',#852,.T.);
#609=FACE_OUTER_BOUND('',#853,.T.);
#610=FACE_OUTER_BOUND('',#854,.T.);
#611=FACE_OUTER_BOUND('',#855,.T.);
#612=FACE_OUTER_BOUND('',#856,.T.);
#613=FACE_OUTER_BOUND('',#857,.T.);
#614=FACE_OUTER_BOUND('',#858,.T.);
#615=FACE_OUTER_BOUND('',#859,.T.);
#616=FACE_OUTER_BOUND('',#860,.T.);
#617=FACE_OUTER_BOUND('',#863,.T.);
#618=FACE_OUTER_BOUND('',#864,.T.);
#619=FACE_OUTER_BOUND('',#865,.T.);
#620=FACE_OUTER_BOUND('',#866,.T.);
#621=FACE_OUTER_BOUND('',#867,.T.);
#622=FACE_OUTER_BOUND('',#868,.T.);
#623=FACE_OUTER_BOUND('',#869,.T.);
#624=FACE_OUTER_BOUND('',#870,.T.);
#625=FACE_OUTER_BOUND('',#871,.T.);
#626=FACE_OUTER_BOUND('',#872,.T.);
#627=FACE_OUTER_BOUND('',#873,.T.);
#628=FACE_OUTER_BOUND('',#874,.T.);
#629=FACE_OUTER_BOUND('',#875,.T.);
#630=FACE_OUTER_BOUND('',#876,.T.);
#631=FACE_OUTER_BOUND('',#877,.T.);
#632=FACE_OUTER_BOUND('',#878,.T.);
#633=FACE_OUTER_BOUND('',#879,.T.);
#634=FACE_OUTER_BOUND('',#880,.T.);
#635=FACE_OUTER_BOUND('',#881,.T.);
#636=FACE_OUTER_BOUND('',#882,.T.);
#637=FACE_OUTER_BOUND('',#883,.T.);
#638=FACE_OUTER_BOUND('',#884,.T.);
#639=FACE_OUTER_BOUND('',#885,.T.);
#640=FACE_OUTER_BOUND('',#886,.T.);
#641=FACE_OUTER_BOUND('',#887,.T.);
#642=FACE_OUTER_BOUND('',#888,.T.);
#643=FACE_OUTER_BOUND('',#889,.T.);
#644=FACE_OUTER_BOUND('',#890,.T.);
#645=FACE_OUTER_BOUND('',#891,.T.);
#646=FACE_OUTER_BOUND('',#892,.T.);
#647=FACE_OUTER_BOUND('',#893,.T.);
#648=FACE_OUTER_BOUND('',#894,.T.);
#649=FACE_OUTER_BOUND('',#895,.T.);
#650=FACE_OUTER_BOUND('',#896,.T.);
#651=FACE_OUTER_BOUND('',#897,.T.);
#652=FACE_OUTER_BOUND('',#898,.T.);
#653=FACE_OUTER_BOUND('',#899,.T.);
#654=FACE_OUTER_BOUND('',#900,.T.);
#655=FACE_OUTER_BOUND('',#901,.T.);
#656=FACE_OUTER_BOUND('',#902,.T.);
#657=FACE_OUTER_BOUND('',#903,.T.);
#658=FACE_OUTER_BOUND('',#904,.T.);
#659=FACE_OUTER_BOUND('',#907,.T.);
#660=FACE_OUTER_BOUND('',#908,.T.);
#661=FACE_OUTER_BOUND('',#909,.T.);
#662=FACE_OUTER_BOUND('',#910,.T.);
#663=FACE_OUTER_BOUND('',#911,.T.);
#664=FACE_OUTER_BOUND('',#912,.T.);
#665=FACE_OUTER_BOUND('',#913,.T.);
#666=FACE_OUTER_BOUND('',#914,.T.);
#667=FACE_OUTER_BOUND('',#915,.T.);
#668=FACE_OUTER_BOUND('',#916,.T.);
#669=FACE_OUTER_BOUND('',#917,.T.);
#670=FACE_OUTER_BOUND('',#918,.T.);
#671=FACE_OUTER_BOUND('',#919,.T.);
#672=FACE_OUTER_BOUND('',#920,.T.);
#673=FACE_OUTER_BOUND('',#921,.T.);
#674=FACE_OUTER_BOUND('',#922,.T.);
#675=FACE_OUTER_BOUND('',#923,.T.);
#676=FACE_OUTER_BOUND('',#924,.T.);
#677=FACE_OUTER_BOUND('',#925,.T.);
#678=FACE_OUTER_BOUND('',#926,.T.);
#679=FACE_OUTER_BOUND('',#929,.T.);
#680=FACE_OUTER_BOUND('',#930,.T.);
#681=FACE_OUTER_BOUND('',#932,.T.);
#682=FACE_OUTER_BOUND('',#933,.T.);
#683=FACE_OUTER_BOUND('',#934,.T.);
#684=FACE_OUTER_BOUND('',#936,.T.);
#685=FACE_OUTER_BOUND('',#937,.T.);
#686=FACE_OUTER_BOUND('',#938,.T.);
#687=FACE_OUTER_BOUND('',#941,.T.);
#688=FACE_OUTER_BOUND('',#942,.T.);
#689=FACE_OUTER_BOUND('',#943,.T.);
#690=FACE_OUTER_BOUND('',#944,.T.);
#691=FACE_OUTER_BOUND('',#945,.T.);
#692=FACE_OUTER_BOUND('',#948,.T.);
#693=FACE_OUTER_BOUND('',#949,.T.);
#694=FACE_OUTER_BOUND('',#950,.T.);
#695=FACE_OUTER_BOUND('',#952,.T.);
#696=FACE_OUTER_BOUND('',#953,.T.);
#697=FACE_OUTER_BOUND('',#954,.T.);
#698=FACE_OUTER_BOUND('',#955,.T.);
#699=FACE_OUTER_BOUND('',#956,.T.);
#700=FACE_OUTER_BOUND('',#957,.T.);
#701=FACE_OUTER_BOUND('',#958,.T.);
#702=FACE_OUTER_BOUND('',#959,.T.);
#703=FACE_OUTER_BOUND('',#960,.T.);
#704=FACE_OUTER_BOUND('',#961,.T.);
#705=FACE_OUTER_BOUND('',#963,.T.);
#706=FACE_OUTER_BOUND('',#964,.T.);
#707=FACE_OUTER_BOUND('',#965,.T.);
#708=FACE_OUTER_BOUND('',#966,.T.);
#709=FACE_OUTER_BOUND('',#967,.T.);
#710=FACE_OUTER_BOUND('',#968,.T.);
#711=FACE_OUTER_BOUND('',#969,.T.);
#712=FACE_OUTER_BOUND('',#970,.T.);
#713=FACE_OUTER_BOUND('',#971,.T.);
#714=FACE_OUTER_BOUND('',#972,.T.);
#715=FACE_OUTER_BOUND('',#973,.T.);
#716=FACE_OUTER_BOUND('',#974,.T.);
#717=FACE_OUTER_BOUND('',#976,.T.);
#718=FACE_OUTER_BOUND('',#977,.T.);
#719=FACE_OUTER_BOUND('',#978,.T.);
#720=FACE_OUTER_BOUND('',#979,.T.);
#721=FACE_OUTER_BOUND('',#980,.T.);
#722=FACE_OUTER_BOUND('',#981,.T.);
#723=FACE_OUTER_BOUND('',#982,.T.);
#724=FACE_OUTER_BOUND('',#983,.T.);
#725=FACE_OUTER_BOUND('',#985,.T.);
#726=FACE_OUTER_BOUND('',#987,.T.);
#727=FACE_OUTER_BOUND('',#988,.T.);
#728=FACE_OUTER_BOUND('',#989,.T.);
#729=FACE_OUTER_BOUND('',#990,.T.);
#730=FACE_OUTER_BOUND('',#991,.T.);
#731=FACE_OUTER_BOUND('',#992,.T.);
#732=FACE_OUTER_BOUND('',#993,.T.);
#733=FACE_OUTER_BOUND('',#994,.T.);
#734=FACE_OUTER_BOUND('',#995,.T.);
#735=FACE_OUTER_BOUND('',#997,.T.);
#736=FACE_OUTER_BOUND('',#998,.T.);
#737=FACE_OUTER_BOUND('',#999,.T.);
#738=FACE_OUTER_BOUND('',#1000,.T.);
#739=FACE_OUTER_BOUND('',#1001,.T.);
#740=FACE_OUTER_BOUND('',#1002,.T.);
#741=FACE_OUTER_BOUND('',#1004,.T.);
#742=FACE_OUTER_BOUND('',#1005,.T.);
#743=FACE_OUTER_BOUND('',#1007,.T.);
#744=FACE_OUTER_BOUND('',#1008,.T.);
#745=FACE_OUTER_BOUND('',#1009,.T.);
#746=FACE_OUTER_BOUND('',#1010,.T.);
#747=FACE_OUTER_BOUND('',#1011,.T.);
#748=FACE_OUTER_BOUND('',#1013,.T.);
#749=FACE_OUTER_BOUND('',#1014,.T.);
#750=FACE_OUTER_BOUND('',#1016,.T.);
#751=FACE_OUTER_BOUND('',#1018,.T.);
#752=FACE_OUTER_BOUND('',#1019,.T.);
#753=FACE_OUTER_BOUND('',#1020,.T.);
#754=FACE_OUTER_BOUND('',#1021,.T.);
#755=FACE_OUTER_BOUND('',#1022,.T.);
#756=FACE_OUTER_BOUND('',#1023,.T.);
#757=FACE_OUTER_BOUND('',#1024,.T.);
#758=FACE_OUTER_BOUND('',#1025,.T.);
#759=FACE_OUTER_BOUND('',#1026,.T.);
#760=FACE_OUTER_BOUND('',#1027,.T.);
#761=EDGE_LOOP('',(#2527,#2528,#2529,#2530));
#762=EDGE_LOOP('',(#2531,#2532,#2533,#2534));
#763=EDGE_LOOP('',(#2535,#2536,#2537,#2538));
#764=EDGE_LOOP('',(#2539,#2540,#2541,#2542));
#765=EDGE_LOOP('',(#2543,#2544,#2545,#2546,#2547,#2548,#2549,#2550));
#766=EDGE_LOOP('',(#2551,#2552,#2553,#2554));
#767=EDGE_LOOP('',(#2555,#2556,#2557,#2558,#2559,#2560,#2561,#2562));
#768=EDGE_LOOP('',(#2563,#2564,#2565,#2566));
#769=EDGE_LOOP('',(#2567,#2568,#2569,#2570,#2571,#2572,#2573,#2574));
#770=EDGE_LOOP('',(#2575));
#771=EDGE_LOOP('',(#2576));
#772=EDGE_LOOP('',(#2577,#2578,#2579,#2580));
#773=EDGE_LOOP('',(#2581,#2582,#2583,#2584,#2585,#2586,#2587,#2588,#2589,
#2590,#2591,#2592,#2593,#2594,#2595,#2596));
#774=EDGE_LOOP('',(#2597,#2598,#2599,#2600,#2601,#2602,#2603,#2604));
#775=EDGE_LOOP('',(#2605));
#776=EDGE_LOOP('',(#2606));
#777=EDGE_LOOP('',(#2607,#2608,#2609,#2610));
#778=EDGE_LOOP('',(#2611,#2612,#2613,#2614));
#779=EDGE_LOOP('',(#2615,#2616,#2617,#2618));
#780=EDGE_LOOP('',(#2619,#2620,#2621));
#781=EDGE_LOOP('',(#2622,#2623,#2624,#2625));
#782=EDGE_LOOP('',(#2626,#2627,#2628,#2629));
#783=EDGE_LOOP('',(#2630,#2631,#2632,#2633));
#784=EDGE_LOOP('',(#2634,#2635,#2636,#2637));
#785=EDGE_LOOP('',(#2638,#2639));
#786=EDGE_LOOP('',(#2640));
#787=EDGE_LOOP('',(#2641,#2642,#2643,#2644,#2645,#2646));
#788=EDGE_LOOP('',(#2647,#2648,#2649,#2650,#2651,#2652,#2653,#2654,#2655,
#2656,#2657,#2658,#2659));
#789=EDGE_LOOP('',(#2660,#2661,#2662,#2663));
#790=EDGE_LOOP('',(#2664,#2665,#2666,#2667));
#791=EDGE_LOOP('',(#2668,#2669,#2670,#2671));
#792=EDGE_LOOP('',(#2672,#2673,#2674,#2675));
#793=EDGE_LOOP('',(#2676,#2677,#2678,#2679));
#794=EDGE_LOOP('',(#2680,#2681,#2682));
#795=EDGE_LOOP('',(#2683,#2684,#2685,#2686));
#796=EDGE_LOOP('',(#2687,#2688));
#797=EDGE_LOOP('',(#2689));
#798=EDGE_LOOP('',(#2690,#2691,#2692,#2693));
#799=EDGE_LOOP('',(#2694,#2695,#2696,#2697,#2698,#2699));
#800=EDGE_LOOP('',(#2700,#2701,#2702));
#801=EDGE_LOOP('',(#2703,#2704,#2705,#2706));
#802=EDGE_LOOP('',(#2707,#2708,#2709,#2710));
#803=EDGE_LOOP('',(#2711,#2712,#2713,#2714,#2715,#2716));
#804=EDGE_LOOP('',(#2717,#2718,#2719,#2720,#2721,#2722));
#805=EDGE_LOOP('',(#2723,#2724,#2725,#2726,#2727));
#806=EDGE_LOOP('',(#2728,#2729,#2730));
#807=EDGE_LOOP('',(#2731,#2732,#2733,#2734,#2735,#2736));
#808=EDGE_LOOP('',(#2737,#2738,#2739,#2740));
#809=EDGE_LOOP('',(#2741,#2742,#2743,#2744));
#810=EDGE_LOOP('',(#2745,#2746,#2747));
#811=EDGE_LOOP('',(#2748,#2749,#2750,#2751,#2752,#2753));
#812=EDGE_LOOP('',(#2754,#2755,#2756,#2757));
#813=EDGE_LOOP('',(#2758,#2759,#2760,#2761,#2762,#2763));
#814=EDGE_LOOP('',(#2764,#2765,#2766));
#815=EDGE_LOOP('',(#2767,#2768));
#816=EDGE_LOOP('',(#2769));
#817=EDGE_LOOP('',(#2770,#2771,#2772,#2773,#2774,#2775));
#818=EDGE_LOOP('',(#2776,#2777,#2778,#2779));
#819=EDGE_LOOP('',(#2780,#2781,#2782,#2783));
#820=EDGE_LOOP('',(#2784,#2785,#2786,#2787));
#821=EDGE_LOOP('',(#2788,#2789,#2790,#2791,#2792));
#822=EDGE_LOOP('',(#2793,#2794,#2795,#2796));
#823=EDGE_LOOP('',(#2797,#2798,#2799,#2800,#2801));
#824=EDGE_LOOP('',(#2802,#2803,#2804,#2805));
#825=EDGE_LOOP('',(#2806,#2807,#2808,#2809));
#826=EDGE_LOOP('',(#2810,#2811,#2812,#2813));
#827=EDGE_LOOP('',(#2814,#2815,#2816));
#828=EDGE_LOOP('',(#2817,#2818,#2819));
#829=EDGE_LOOP('',(#2820,#2821,#2822,#2823,#2824,#2825));
#830=EDGE_LOOP('',(#2826,#2827,#2828,#2829,#2830,#2831,#2832,#2833,#2834,
#2835,#2836,#2837,#2838));
#831=EDGE_LOOP('',(#2839,#2840,#2841,#2842));
#832=EDGE_LOOP('',(#2843,#2844,#2845,#2846));
#833=EDGE_LOOP('',(#2847,#2848,#2849,#2850,#2851));
#834=EDGE_LOOP('',(#2852,#2853,#2854,#2855));
#835=EDGE_LOOP('',(#2856,#2857,#2858,#2859,#2860));
#836=EDGE_LOOP('',(#2861,#2862,#2863,#2864));
#837=EDGE_LOOP('',(#2865,#2866,#2867,#2868));
#838=EDGE_LOOP('',(#2869,#2870,#2871,#2872,#2873,#2874,#2875,#2876,#2877,
#2878,#2879,#2880,#2881,#2882));
#839=EDGE_LOOP('',(#2883));
#840=EDGE_LOOP('',(#2884,#2885,#2886,#2887,#2888));
#841=EDGE_LOOP('',(#2889,#2890,#2891,#2892,#2893,#2894));
#842=EDGE_LOOP('',(#2895,#2896,#2897,#2898));
#843=EDGE_LOOP('',(#2899,#2900,#2901,#2902,#2903,#2904));
#844=EDGE_LOOP('',(#2905,#2906));
#845=EDGE_LOOP('',(#2907));
#846=EDGE_LOOP('',(#2908,#2909,#2910,#2911,#2912,#2913));
#847=EDGE_LOOP('',(#2914,#2915,#2916,#2917));
#848=EDGE_LOOP('',(#2918,#2919,#2920,#2921,#2922,#2923));
#849=EDGE_LOOP('',(#2924,#2925,#2926,#2927));
#850=EDGE_LOOP('',(#2928,#2929,#2930,#2931));
#851=EDGE_LOOP('',(#2932,#2933,#2934,#2935));
#852=EDGE_LOOP('',(#2936,#2937,#2938,#2939,#2940));
#853=EDGE_LOOP('',(#2941,#2942,#2943));
#854=EDGE_LOOP('',(#2944,#2945,#2946,#2947));
#855=EDGE_LOOP('',(#2948,#2949,#2950));
#856=EDGE_LOOP('',(#2951,#2952,#2953,#2954));
#857=EDGE_LOOP('',(#2955,#2956,#2957,#2958));
#858=EDGE_LOOP('',(#2959,#2960,#2961,#2962,#2963,#2964));
#859=EDGE_LOOP('',(#2965,#2966,#2967,#2968));
#860=EDGE_LOOP('',(#2969,#2970,#2971,#2972,#2973,#2974,#2975,#2976));
#861=EDGE_LOOP('',(#2977));
#862=EDGE_LOOP('',(#2978));
#863=EDGE_LOOP('',(#2979,#2980,#2981,#2982,#2983,#2984,#2985,#2986,#2987,
#2988,#2989,#2990,#2991,#2992,#2993,#2994,#2995,#2996,#2997,#2998,#2999,
#3000,#3001,#3002));
#864=EDGE_LOOP('',(#3003,#3004,#3005,#3006));
#865=EDGE_LOOP('',(#3007));
#866=EDGE_LOOP('',(#3008,#3009,#3010,#3011));
#867=EDGE_LOOP('',(#3012));
#868=EDGE_LOOP('',(#3013,#3014,#3015,#3016));
#869=EDGE_LOOP('',(#3017,#3018,#3019,#3020));
#870=EDGE_LOOP('',(#3021,#3022,#3023,#3024));
#871=EDGE_LOOP('',(#3025,#3026,#3027,#3028));
#872=EDGE_LOOP('',(#3029,#3030,#3031,#3032));
#873=EDGE_LOOP('',(#3033,#3034,#3035,#3036));
#874=EDGE_LOOP('',(#3037,#3038,#3039,#3040));
#875=EDGE_LOOP('',(#3041,#3042,#3043,#3044));
#876=EDGE_LOOP('',(#3045,#3046,#3047,#3048));
#877=EDGE_LOOP('',(#3049,#3050,#3051,#3052));
#878=EDGE_LOOP('',(#3053,#3054,#3055,#3056));
#879=EDGE_LOOP('',(#3057,#3058,#3059,#3060,#3061,#3062));
#880=EDGE_LOOP('',(#3063,#3064,#3065,#3066,#3067,#3068));
#881=EDGE_LOOP('',(#3069,#3070,#3071,#3072,#3073,#3074));
#882=EDGE_LOOP('',(#3075,#3076,#3077,#3078));
#883=EDGE_LOOP('',(#3079,#3080,#3081,#3082));
#884=EDGE_LOOP('',(#3083,#3084,#3085,#3086));
#885=EDGE_LOOP('',(#3087,#3088,#3089,#3090));
#886=EDGE_LOOP('',(#3091,#3092,#3093,#3094));
#887=EDGE_LOOP('',(#3095,#3096,#3097,#3098));
#888=EDGE_LOOP('',(#3099,#3100,#3101,#3102));
#889=EDGE_LOOP('',(#3103,#3104,#3105,#3106));
#890=EDGE_LOOP('',(#3107,#3108,#3109,#3110));
#891=EDGE_LOOP('',(#3111,#3112,#3113,#3114,#3115,#3116,#3117));
#892=EDGE_LOOP('',(#3118,#3119,#3120,#3121,#3122));
#893=EDGE_LOOP('',(#3123,#3124,#3125,#3126));
#894=EDGE_LOOP('',(#3127,#3128,#3129,#3130));
#895=EDGE_LOOP('',(#3131,#3132,#3133,#3134,#3135,#3136));
#896=EDGE_LOOP('',(#3137,#3138,#3139,#3140));
#897=EDGE_LOOP('',(#3141,#3142,#3143,#3144));
#898=EDGE_LOOP('',(#3145,#3146,#3147,#3148,#3149,#3150));
#899=EDGE_LOOP('',(#3151,#3152,#3153,#3154,#3155));
#900=EDGE_LOOP('',(#3156,#3157,#3158,#3159,#3160));
#901=EDGE_LOOP('',(#3161,#3162,#3163,#3164,#3165,#3166,#3167));
#902=EDGE_LOOP('',(#3168,#3169,#3170,#3171));
#903=EDGE_LOOP('',(#3172,#3173,#3174,#3175,#3176,#3177));
#904=EDGE_LOOP('',(#3178,#3179,#3180,#3181,#3182,#3183));
#905=EDGE_LOOP('',(#3184));
#906=EDGE_LOOP('',(#3185));
#907=EDGE_LOOP('',(#3186,#3187,#3188,#3189,#3190,#3191,#3192,#3193));
#908=EDGE_LOOP('',(#3194,#3195,#3196,#3197));
#909=EDGE_LOOP('',(#3198,#3199,#3200,#3201));
#910=EDGE_LOOP('',(#3202,#3203,#3204,#3205,#3206,#3207,#3208,#3209));
#911=EDGE_LOOP('',(#3210,#3211,#3212,#3213,#3214));
#912=EDGE_LOOP('',(#3215,#3216,#3217,#3218,#3219,#3220,#3221));
#913=EDGE_LOOP('',(#3222,#3223,#3224,#3225));
#914=EDGE_LOOP('',(#3226,#3227,#3228,#3229));
#915=EDGE_LOOP('',(#3230,#3231,#3232));
#916=EDGE_LOOP('',(#3233,#3234,#3235,#3236));
#917=EDGE_LOOP('',(#3237,#3238,#3239,#3240));
#918=EDGE_LOOP('',(#3241));
#919=EDGE_LOOP('',(#3242,#3243,#3244,#3245));
#920=EDGE_LOOP('',(#3246,#3247,#3248,#3249));
#921=EDGE_LOOP('',(#3250,#3251,#3252,#3253,#3254,#3255,#3256,#3257));
#922=EDGE_LOOP('',(#3258,#3259,#3260,#3261));
#923=EDGE_LOOP('',(#3262,#3263,#3264,#3265));
#924=EDGE_LOOP('',(#3266,#3267,#3268,#3269,#3270,#3271,#3272));
#925=EDGE_LOOP('',(#3273,#3274,#3275,#3276));
#926=EDGE_LOOP('',(#3277,#3278,#3279,#3280,#3281,#3282,#3283,#3284,#3285,
#3286,#3287,#3288,#3289,#3290,#3291,#3292,#3293,#3294,#3295,#3296,#3297,
#3298));
#927=EDGE_LOOP('',(#3299));
#928=EDGE_LOOP('',(#3300));
#929=EDGE_LOOP('',(#3301,#3302,#3303,#3304));
#930=EDGE_LOOP('',(#3305));
#931=EDGE_LOOP('',(#3306));
#932=EDGE_LOOP('',(#3307,#3308,#3309,#3310));
#933=EDGE_LOOP('',(#3311,#3312,#3313,#3314));
#934=EDGE_LOOP('',(#3315));
#935=EDGE_LOOP('',(#3316));
#936=EDGE_LOOP('',(#3317,#3318,#3319,#3320));
#937=EDGE_LOOP('',(#3321,#3322,#3323,#3324));
#938=EDGE_LOOP('',(#3325,#3326,#3327,#3328));
#939=EDGE_LOOP('',(#3329));
#940=EDGE_LOOP('',(#3330));
#941=EDGE_LOOP('',(#3331,#3332,#3333,#3334));
#942=EDGE_LOOP('',(#3335,#3336,#3337,#3338));
#943=EDGE_LOOP('',(#3339,#3340,#3341,#3342));
#944=EDGE_LOOP('',(#3343,#3344,#3345,#3346));
#945=EDGE_LOOP('',(#3347,#3348,#3349,#3350));
#946=EDGE_LOOP('',(#3351));
#947=EDGE_LOOP('',(#3352));
#948=EDGE_LOOP('',(#3353,#3354,#3355,#3356,#3357));
#949=EDGE_LOOP('',(#3358,#3359,#3360,#3361,#3362));
#950=EDGE_LOOP('',(#3363));
#951=EDGE_LOOP('',(#3364));
#952=EDGE_LOOP('',(#3365,#3366,#3367,#3368));
#953=EDGE_LOOP('',(#3369,#3370,#3371,#3372));
#954=EDGE_LOOP('',(#3373,#3374,#3375,#3376));
#955=EDGE_LOOP('',(#3377,#3378,#3379,#3380));
#956=EDGE_LOOP('',(#3381,#3382,#3383,#3384));
#957=EDGE_LOOP('',(#3385,#3386,#3387,#3388));
#958=EDGE_LOOP('',(#3389,#3390,#3391,#3392,#3393,#3394));
#959=EDGE_LOOP('',(#3395,#3396,#3397,#3398,#3399));
#960=EDGE_LOOP('',(#3400,#3401,#3402,#3403,#3404));
#961=EDGE_LOOP('',(#3405));
#962=EDGE_LOOP('',(#3406,#3407,#3408,#3409,#3410,#3411));
#963=EDGE_LOOP('',(#3412));
#964=EDGE_LOOP('',(#3413,#3414,#3415,#3416));
#965=EDGE_LOOP('',(#3417,#3418,#3419,#3420));
#966=EDGE_LOOP('',(#3421,#3422,#3423,#3424));
#967=EDGE_LOOP('',(#3425,#3426,#3427,#3428));
#968=EDGE_LOOP('',(#3429,#3430,#3431,#3432));
#969=EDGE_LOOP('',(#3433,#3434,#3435,#3436));
#970=EDGE_LOOP('',(#3437,#3438,#3439,#3440,#3441,#3442));
#971=EDGE_LOOP('',(#3443,#3444,#3445,#3446));
#972=EDGE_LOOP('',(#3447,#3448,#3449,#3450,#3451,#3452,#3453,#3454,#3455,
#3456,#3457,#3458));
#973=EDGE_LOOP('',(#3459,#3460,#3461,#3462,#3463,#3464,#3465,#3466,#3467,
#3468,#3469,#3470));
#974=EDGE_LOOP('',(#3471));
#975=EDGE_LOOP('',(#3472));
#976=EDGE_LOOP('',(#3473,#3474,#3475,#3476));
#977=EDGE_LOOP('',(#3477,#3478,#3479,#3480));
#978=EDGE_LOOP('',(#3481,#3482,#3483,#3484));
#979=EDGE_LOOP('',(#3485,#3486,#3487,#3488));
#980=EDGE_LOOP('',(#3489,#3490,#3491,#3492));
#981=EDGE_LOOP('',(#3493,#3494,#3495,#3496));
#982=EDGE_LOOP('',(#3497,#3498,#3499,#3500));
#983=EDGE_LOOP('',(#3501,#3502,#3503,#3504,#3505,#3506));
#984=EDGE_LOOP('',(#3507));
#985=EDGE_LOOP('',(#3508,#3509,#3510,#3511,#3512,#3513));
#986=EDGE_LOOP('',(#3514));
#987=EDGE_LOOP('',(#3515,#3516,#3517,#3518));
#988=EDGE_LOOP('',(#3519,#3520,#3521,#3522));
#989=EDGE_LOOP('',(#3523,#3524,#3525,#3526));
#990=EDGE_LOOP('',(#3527,#3528,#3529));
#991=EDGE_LOOP('',(#3530,#3531));
#992=EDGE_LOOP('',(#3532,#3533,#3534,#3535));
#993=EDGE_LOOP('',(#3536));
#994=EDGE_LOOP('',(#3537,#3538,#3539,#3540,#3541,#3542,#3543,#3544,#3545,
#3546,#3547,#3548));
#995=EDGE_LOOP('',(#3549));
#996=EDGE_LOOP('',(#3550));
#997=EDGE_LOOP('',(#3551,#3552,#3553,#3554,#3555));
#998=EDGE_LOOP('',(#3556,#3557,#3558,#3559,#3560,#3561));
#999=EDGE_LOOP('',(#3562));
#1000=EDGE_LOOP('',(#3563,#3564,#3565,#3566,#3567,#3568));
#1001=EDGE_LOOP('',(#3569,#3570,#3571,#3572,#3573));
#1002=EDGE_LOOP('',(#3574));
#1003=EDGE_LOOP('',(#3575));
#1004=EDGE_LOOP('',(#3576,#3577,#3578,#3579));
#1005=EDGE_LOOP('',(#3580));
#1006=EDGE_LOOP('',(#3581));
#1007=EDGE_LOOP('',(#3582,#3583,#3584,#3585));
#1008=EDGE_LOOP('',(#3586));
#1009=EDGE_LOOP('',(#3587,#3588,#3589,#3590));
#1010=EDGE_LOOP('',(#3591,#3592,#3593,#3594));
#1011=EDGE_LOOP('',(#3595));
#1012=EDGE_LOOP('',(#3596));
#1013=EDGE_LOOP('',(#3597,#3598,#3599,#3600));
#1014=EDGE_LOOP('',(#3601));
#1015=EDGE_LOOP('',(#3602));
#1016=EDGE_LOOP('',(#3603));
#1017=EDGE_LOOP('',(#3604));
#1018=EDGE_LOOP('',(#3605,#3606,#3607,#3608));
#1019=EDGE_LOOP('',(#3609,#3610,#3611,#3612));
#1020=EDGE_LOOP('',(#3613,#3614,#3615,#3616));
#1021=EDGE_LOOP('',(#3617,#3618,#3619,#3620));
#1022=EDGE_LOOP('',(#3621,#3622,#3623,#3624));
#1023=EDGE_LOOP('',(#3625,#3626,#3627,#3628));
#1024=EDGE_LOOP('',(#3629,#3630,#3631,#3632));
#1025=EDGE_LOOP('',(#3633,#3634,#3635,#3636));
#1026=EDGE_LOOP('',(#3637,#3638,#3639,#3640,#3641,#3642,#3643,#3644));
#1027=EDGE_LOOP('',(#3645,#3646,#3647,#3648,#3649,#3650,#3651,#3652));
#1028=LINE('',#5611,#1317);
#1029=LINE('',#5613,#1318);
#1030=LINE('',#5615,#1319);
#1031=LINE('',#5616,#1320);
#1032=LINE('',#5619,#1321);
#1033=LINE('',#5621,#1322);
#1034=LINE('',#5622,#1323);
#1035=LINE('',#5626,#1324);
#1036=LINE('',#5628,#1325);
#1037=LINE('',#5630,#1326);
#1038=LINE('',#5631,#1327);
#1039=LINE('',#5635,#1328);
#1040=LINE('',#5637,#1329);
#1041=LINE('',#5639,#1330);
#1042=LINE('',#5640,#1331);
#1043=LINE('',#5643,#1332);
#1044=LINE('',#5645,#1333);
#1045=LINE('',#5647,#1334);
#1046=LINE('',#5649,#1335);
#1047=LINE('',#5650,#1336);
#1048=LINE('',#5651,#1337);
#1049=LINE('',#5654,#1338);
#1050=LINE('',#5656,#1339);
#1051=LINE('',#5657,#1340);
#1052=LINE('',#5660,#1341);
#1053=LINE('',#5661,#1342);
#1054=LINE('',#5663,#1343);
#1055=LINE('',#5665,#1344);
#1056=LINE('',#5667,#1345);
#1057=LINE('',#5668,#1346);
#1058=LINE('',#5670,#1347);
#1059=LINE('',#5671,#1348);
#1060=LINE('',#5674,#1349);
#1061=LINE('',#5676,#1350);
#1062=LINE('',#5678,#1351);
#1063=LINE('',#5680,#1352);
#1064=LINE('',#5681,#1353);
#1065=LINE('',#5688,#1354);
#1066=LINE('',#5689,#1355);
#1067=LINE('',#5692,#1356);
#1068=LINE('',#5694,#1357);
#1069=LINE('',#5698,#1358);
#1070=LINE('',#5700,#1359);
#1071=LINE('',#5702,#1360);
#1072=LINE('',#5706,#1361);
#1073=LINE('',#5707,#1362);
#1074=LINE('',#5710,#1363);
#1075=LINE('',#5716,#1364);
#1076=LINE('',#5856,#1365);
#1077=LINE('',#5861,#1366);
#1078=LINE('',#5864,#1367);
#1079=LINE('',#5866,#1368);
#1080=LINE('',#5870,#1369);
#1081=LINE('',#5872,#1370);
#1082=LINE('',#5874,#1371);
#1083=LINE('',#5876,#1372);
#1084=LINE('',#5878,#1373);
#1085=LINE('',#5880,#1374);
#1086=LINE('',#5882,#1375);
#1087=LINE('',#5883,#1376);
#1088=LINE('',#5908,#1377);
#1089=LINE('',#6015,#1378);
#1090=LINE('',#6019,#1379);
#1091=LINE('',#6020,#1380);
#1092=LINE('',#6152,#1381);
#1093=LINE('',#6155,#1382);
#1094=LINE('',#6158,#1383);
#1095=LINE('',#6166,#1384);
#1096=LINE('',#6339,#1385);
#1097=LINE('',#6340,#1386);
#1098=LINE('',#6342,#1387);
#1099=LINE('',#6345,#1388);
#1100=LINE('',#6348,#1389);
#1101=LINE('',#6395,#1390);
#1102=LINE('',#6398,#1391);
#1103=LINE('',#6423,#1392);
#1104=LINE('',#6424,#1393);
#1105=LINE('',#6609,#1394);
#1106=LINE('',#6610,#1395);
#1107=LINE('',#6613,#1396);
#1108=LINE('',#6619,#1397);
#1109=LINE('',#6621,#1398);
#1110=LINE('',#6623,#1399);
#1111=LINE('',#6625,#1400);
#1112=LINE('',#6626,#1401);
#1113=LINE('',#6627,#1402);
#1114=LINE('',#6630,#1403);
#1115=LINE('',#6634,#1404);
#1116=LINE('',#6635,#1405);
#1117=LINE('',#6638,#1406);
#1118=LINE('',#6642,#1407);
#1119=LINE('',#6646,#1408);
#1120=LINE('',#6650,#1409);
#1121=LINE('',#6651,#1410);
#1122=LINE('',#6655,#1411);
#1123=LINE('',#6663,#1412);
#1124=LINE('',#6665,#1413);
#1125=LINE('',#6666,#1414);
#1126=LINE('',#6670,#1415);
#1127=LINE('',#6677,#1416);
#1128=LINE('',#6682,#1417);
#1129=LINE('',#6685,#1418);
#1130=LINE('',#6688,#1419);
#1131=LINE('',#6690,#1420);
#1132=LINE('',#6695,#1421);
#1133=LINE('',#6697,#1422);
#1134=LINE('',#6702,#1423);
#1135=LINE('',#6704,#1424);
#1136=LINE('',#6707,#1425);
#1137=LINE('',#6710,#1426);
#1138=LINE('',#6717,#1427);
#1139=LINE('',#6724,#1428);
#1140=LINE('',#7338,#1429);
#1141=LINE('',#7351,#1430);
#1142=LINE('',#7352,#1431);
#1143=LINE('',#7355,#1432);
#1144=LINE('',#7359,#1433);
#1145=LINE('',#7362,#1434);
#1146=LINE('',#7881,#1435);
#1147=LINE('',#7884,#1436);
#1148=LINE('',#7885,#1437);
#1149=LINE('',#7887,#1438);
#1150=LINE('',#7889,#1439);
#1151=LINE('',#7891,#1440);
#1152=LINE('',#7893,#1441);
#1153=LINE('',#7895,#1442);
#1154=LINE('',#7897,#1443);
#1155=LINE('',#7900,#1444);
#1156=LINE('',#7903,#1445);
#1157=LINE('',#7906,#1446);
#1158=LINE('',#7909,#1447);
#1159=LINE('',#7912,#1448);
#1160=LINE('',#7914,#1449);
#1161=LINE('',#7915,#1450);
#1162=LINE('',#7918,#1451);
#1163=LINE('',#7919,#1452);
#1164=LINE('',#7922,#1453);
#1165=LINE('',#7923,#1454);
#1166=LINE('',#7925,#1455);
#1167=LINE('',#7927,#1456);
#1168=LINE('',#7932,#1457);
#1169=LINE('',#7935,#1458);
#1170=LINE('',#7938,#1459);
#1171=LINE('',#7940,#1460);
#1172=LINE('',#7941,#1461);
#1173=LINE('',#7946,#1462);
#1174=LINE('',#7950,#1463);
#1175=LINE('',#7952,#1464);
#1176=LINE('',#7954,#1465);
#1177=LINE('',#7956,#1466);
#1178=LINE('',#7958,#1467);
#1179=LINE('',#7960,#1468);
#1180=LINE('',#7961,#1469);
#1181=LINE('',#7964,#1470);
#1182=LINE('',#7965,#1471);
#1183=LINE('',#7968,#1472);
#1184=LINE('',#7969,#1473);
#1185=LINE('',#7972,#1474);
#1186=LINE('',#7973,#1475);
#1187=LINE('',#7976,#1476);
#1188=LINE('',#7977,#1477);
#1189=LINE('',#7982,#1478);
#1190=LINE('',#7986,#1479);
#1191=LINE('',#7991,#1480);
#1192=LINE('',#7997,#1481);
#1193=LINE('',#7999,#1482);
#1194=LINE('',#8001,#1483);
#1195=LINE('',#8002,#1484);
#1196=LINE('',#8005,#1485);
#1197=LINE('',#8007,#1486);
#1198=LINE('',#8008,#1487);
#1199=LINE('',#8011,#1488);
#1200=LINE('',#8012,#1489);
#1201=LINE('',#8014,#1490);
#1202=LINE('',#8016,#1491);
#1203=LINE('',#8017,#1492);
#1204=LINE('',#8020,#1493);
#1205=LINE('',#8021,#1494);
#1206=LINE('',#8024,#1495);
#1207=LINE('',#8025,#1496);
#1208=LINE('',#8027,#1497);
#1209=LINE('',#8029,#1498);
#1210=LINE('',#8030,#1499);
#1211=LINE('',#8042,#1500);
#1212=LINE('',#8045,#1501);
#1213=LINE('',#8055,#1502);
#1214=LINE('',#8058,#1503);
#1215=LINE('',#8063,#1504);
#1216=LINE('',#8065,#1505);
#1217=LINE('',#8067,#1506);
#1218=LINE('',#8068,#1507);
#1219=LINE('',#8071,#1508);
#1220=LINE('',#8073,#1509);
#1221=LINE('',#8074,#1510);
#1222=LINE('',#8077,#1511);
#1223=LINE('',#8078,#1512);
#1224=LINE('',#8081,#1513);
#1225=LINE('',#8082,#1514);
#1226=LINE('',#8084,#1515);
#1227=LINE('',#8098,#1516);
#1228=LINE('',#8105,#1517);
#1229=LINE('',#8107,#1518);
#1230=LINE('',#8109,#1519);
#1231=LINE('',#8110,#1520);
#1232=LINE('',#8113,#1521);
#1233=LINE('',#8115,#1522);
#1234=LINE('',#8116,#1523);
#1235=LINE('',#8119,#1524);
#1236=LINE('',#8121,#1525);
#1237=LINE('',#8122,#1526);
#1238=LINE('',#8125,#1527);
#1239=LINE('',#8127,#1528);
#1240=LINE('',#8128,#1529);
#1241=LINE('',#8131,#1530);
#1242=LINE('',#8133,#1531);
#1243=LINE('',#8134,#1532);
#1244=LINE('',#8136,#1533);
#1245=LINE('',#8137,#1534);
#1246=LINE('',#8148,#1535);
#1247=LINE('',#8157,#1536);
#1248=LINE('',#8160,#1537);
#1249=LINE('',#8163,#1538);
#1250=LINE('',#8165,#1539);
#1251=LINE('',#8166,#1540);
#1252=LINE('',#8170,#1541);
#1253=LINE('',#8172,#1542);
#1254=LINE('',#8174,#1543);
#1255=LINE('',#8175,#1544);
#1256=LINE('',#8178,#1545);
#1257=LINE('',#8180,#1546);
#1258=LINE('',#8181,#1547);
#1259=LINE('',#8185,#1548);
#1260=LINE('',#8187,#1549);
#1261=LINE('',#8189,#1550);
#1262=LINE('',#8190,#1551);
#1263=LINE('',#8206,#1552);
#1264=LINE('',#8210,#1553);
#1265=LINE('',#8218,#1554);
#1266=LINE('',#8225,#1555);
#1267=LINE('',#8228,#1556);
#1268=LINE('',#8231,#1557);
#1269=LINE('',#8233,#1558);
#1270=LINE('',#8234,#1559);
#1271=LINE('',#8240,#1560);
#1272=LINE('',#8246,#1561);
#1273=LINE('',#8252,#1562);
#1274=LINE('',#8254,#1563);
#1275=LINE('',#8255,#1564);
#1276=LINE('',#8262,#1565);
#1277=LINE('',#8264,#1566);
#1278=LINE('',#8266,#1567);
#1279=LINE('',#8267,#1568);
#1280=LINE('',#8271,#1569);
#1281=LINE('',#8273,#1570);
#1282=LINE('',#8275,#1571);
#1283=LINE('',#8276,#1572);
#1284=LINE('',#8290,#1573);
#1285=LINE('',#8296,#1574);
#1286=LINE('',#8309,#1575);
#1287=LINE('',#8322,#1576);
#1288=LINE('',#8329,#1577);
#1289=LINE('',#8339,#1578);
#1290=LINE('',#8343,#1579);
#1291=LINE('',#8349,#1580);
#1292=LINE('',#8356,#1581);
#1293=LINE('',#8364,#1582);
#1294=LINE('',#8366,#1583);
#1295=LINE('',#8368,#1584);
#1296=LINE('',#8369,#1585);
#1297=LINE('',#8372,#1586);
#1298=LINE('',#8374,#1587);
#1299=LINE('',#8375,#1588);
#1300=LINE('',#8378,#1589);
#1301=LINE('',#8380,#1590);
#1302=LINE('',#8381,#1591);
#1303=LINE('',#8384,#1592);
#1304=LINE('',#8386,#1593);
#1305=LINE('',#8387,#1594);
#1306=LINE('',#8390,#1595);
#1307=LINE('',#8392,#1596);
#1308=LINE('',#8393,#1597);
#1309=LINE('',#8396,#1598);
#1310=LINE('',#8398,#1599);
#1311=LINE('',#8399,#1600);
#1312=LINE('',#8402,#1601);
#1313=LINE('',#8404,#1602);
#1314=LINE('',#8405,#1603);
#1315=LINE('',#8407,#1604);
#1316=LINE('',#8408,#1605);
#1317=VECTOR('',#4519,10.);
#1318=VECTOR('',#4520,10.);
#1319=VECTOR('',#4521,10.);
#1320=VECTOR('',#4522,10.);
#1321=VECTOR('',#4525,10.);
#1322=VECTOR('',#4526,10.);
#1323=VECTOR('',#4527,10.);
#1324=VECTOR('',#4530,10.);
#1325=VECTOR('',#4531,10.);
#1326=VECTOR('',#4532,10.);
#1327=VECTOR('',#4533,10.);
#1328=VECTOR('',#4536,10.);
#1329=VECTOR('',#4537,10.);
#1330=VECTOR('',#4538,10.);
#1331=VECTOR('',#4539,10.);
#1332=VECTOR('',#4542,10.);
#1333=VECTOR('',#4543,10.);
#1334=VECTOR('',#4544,10.);
#1335=VECTOR('',#4545,10.);
#1336=VECTOR('',#4546,10.);
#1337=VECTOR('',#4547,10.);
#1338=VECTOR('',#4550,10.);
#1339=VECTOR('',#4551,10.);
#1340=VECTOR('',#4552,10.);
#1341=VECTOR('',#4555,10.);
#1342=VECTOR('',#4556,10.);
#1343=VECTOR('',#4557,10.);
#1344=VECTOR('',#4558,10.);
#1345=VECTOR('',#4559,10.);
#1346=VECTOR('',#4560,10.);
#1347=VECTOR('',#4563,10.);
#1348=VECTOR('',#4564,10.);
#1349=VECTOR('',#4567,10.);
#1350=VECTOR('',#4568,10.);
#1351=VECTOR('',#4569,10.);
#1352=VECTOR('',#4570,10.);
#1353=VECTOR('',#4571,10.);
#1354=VECTOR('',#4578,10.);
#1355=VECTOR('',#4579,10.);
#1356=VECTOR('',#4582,10.);
#1357=VECTOR('',#4583,10.);
#1358=VECTOR('',#4586,10.);
#1359=VECTOR('',#4587,10.);
#1360=VECTOR('',#4588,10.);
#1361=VECTOR('',#4591,10.);
#1362=VECTOR('',#4592,10.);
#1363=VECTOR('',#4595,10.);
#1364=VECTOR('',#4600,10.);
#1365=VECTOR('',#4639,10.);
#1366=VECTOR('',#4646,10.);
#1367=VECTOR('',#4649,10.);
#1368=VECTOR('',#4652,10.);
#1369=VECTOR('',#4657,10.);
#1370=VECTOR('',#4660,10.);
#1371=VECTOR('',#4661,10.);
#1372=VECTOR('',#4662,10.);
#1373=VECTOR('',#4663,10.);
#1374=VECTOR('',#4664,10.);
#1375=VECTOR('',#4665,10.);
#1376=VECTOR('',#4666,10.);
#1377=VECTOR('',#4679,10.);
#1378=VECTOR('',#4704,10.);
#1379=VECTOR('',#4709,10.);
#1380=VECTOR('',#4710,10.);
#1381=VECTOR('',#4731,10.);
#1382=VECTOR('',#4734,10.);
#1383=VECTOR('',#4737,10.);
#1384=VECTOR('',#4738,10.);
#1385=VECTOR('',#4765,10.);
#1386=VECTOR('',#4766,10.);
#1387=VECTOR('',#4769,10.);
#1388=VECTOR('',#4772,10.);
#1389=VECTOR('',#4775,10.);
#1390=VECTOR('',#4786,10.);
#1391=VECTOR('',#4789,10.);
#1392=VECTOR('',#4802,10.);
#1393=VECTOR('',#4803,10.);
#1394=VECTOR('',#4832,10.);
#1395=VECTOR('',#4833,10.);
#1396=VECTOR('',#4838,10.);
#1397=VECTOR('',#4849,10.);
#1398=VECTOR('',#4852,10.);
#1399=VECTOR('',#4853,10.);
#1400=VECTOR('',#4854,10.);
#1401=VECTOR('',#4855,10.);
#1402=VECTOR('',#4856,10.);
#1403=VECTOR('',#4859,10.);
#1404=VECTOR('',#4864,10.);
#1405=VECTOR('',#4865,10.);
#1406=VECTOR('',#4868,10.);
#1407=VECTOR('',#4873,10.);
#1408=VECTOR('',#4878,10.);
#1409=VECTOR('',#4883,10.);
#1410=VECTOR('',#4884,10.);
#1411=VECTOR('',#4891,10.);
#1412=VECTOR('',#4900,9.5);
#1413=VECTOR('',#4903,10.);
#1414=VECTOR('',#4904,10.);
#1415=VECTOR('',#4911,10.);
#1416=VECTOR('',#4920,4.);
#1417=VECTOR('',#4929,4.);
#1418=VECTOR('',#4932,3.99999999999999);
#1419=VECTOR('',#4937,3.99999999999999);
#1420=VECTOR('',#4940,10.);
#1421=VECTOR('',#4945,1.5);
#1422=VECTOR('',#4948,3.);
#1423=VECTOR('',#4953,1.5);
#1424=VECTOR('',#4956,3.);
#1425=VECTOR('',#4961,10.);
#1426=VECTOR('',#4966,10.);
#1427=VECTOR('',#4975,3.);
#1428=VECTOR('',#4984,3.);
#1429=VECTOR('',#4989,10.);
#1430=VECTOR('',#4992,10.);
#1431=VECTOR('',#4993,10.);
#1432=VECTOR('',#4996,10.);
#1433=VECTOR('',#4999,10.);
#1434=VECTOR('',#5004,10.);
#1435=VECTOR('',#5007,10.);
#1436=VECTOR('',#5010,10.);
#1437=VECTOR('',#5011,10.);
#1438=VECTOR('',#5014,10.);
#1439=VECTOR('',#5017,10.);
#1440=VECTOR('',#5020,10.);
#1441=VECTOR('',#5023,10.);
#1442=VECTOR('',#5026,10.);
#1443=VECTOR('',#5029,10.);
#1444=VECTOR('',#5032,10.);
#1445=VECTOR('',#5035,10.);
#1446=VECTOR('',#5038,10.);
#1447=VECTOR('',#5041,10.);
#1448=VECTOR('',#5044,10.);
#1449=VECTOR('',#5045,10.);
#1450=VECTOR('',#5046,10.);
#1451=VECTOR('',#5049,10.);
#1452=VECTOR('',#5050,10.);
#1453=VECTOR('',#5053,10.);
#1454=VECTOR('',#5054,10.);
#1455=VECTOR('',#5057,10.);
#1456=VECTOR('',#5060,10.);
#1457=VECTOR('',#5065,10.);
#1458=VECTOR('',#5068,10.);
#1459=VECTOR('',#5071,10.);
#1460=VECTOR('',#5072,10.);
#1461=VECTOR('',#5073,10.);
#1462=VECTOR('',#5078,10.);
#1463=VECTOR('',#5083,10.);
#1464=VECTOR('',#5084,10.);
#1465=VECTOR('',#5085,10.);
#1466=VECTOR('',#5086,10.);
#1467=VECTOR('',#5087,10.);
#1468=VECTOR('',#5088,10.);
#1469=VECTOR('',#5089,10.);
#1470=VECTOR('',#5092,10.);
#1471=VECTOR('',#5093,10.);
#1472=VECTOR('',#5096,10.);
#1473=VECTOR('',#5097,10.);
#1474=VECTOR('',#5100,10.);
#1475=VECTOR('',#5101,10.);
#1476=VECTOR('',#5104,10.);
#1477=VECTOR('',#5105,10.);
#1478=VECTOR('',#5110,0.5);
#1479=VECTOR('',#5115,1.);
#1480=VECTOR('',#5120,9.5);
#1481=VECTOR('',#5127,10.);
#1482=VECTOR('',#5128,10.);
#1483=VECTOR('',#5129,10.);
#1484=VECTOR('',#5130,10.);
#1485=VECTOR('',#5133,10.);
#1486=VECTOR('',#5134,10.);
#1487=VECTOR('',#5135,10.);
#1488=VECTOR('',#5138,10.);
#1489=VECTOR('',#5139,10.);
#1490=VECTOR('',#5140,10.);
#1491=VECTOR('',#5141,10.);
#1492=VECTOR('',#5142,10.);
#1493=VECTOR('',#5145,10.);
#1494=VECTOR('',#5146,10.);
#1495=VECTOR('',#5149,10.);
#1496=VECTOR('',#5150,10.);
#1497=VECTOR('',#5153,10.);
#1498=VECTOR('',#5156,10.);
#1499=VECTOR('',#5157,10.);
#1500=VECTOR('',#5174,5.25);
#1501=VECTOR('',#5177,3.25);
#1502=VECTOR('',#5190,5.25);
#1503=VECTOR('',#5193,3.25);
#1504=VECTOR('',#5198,10.);
#1505=VECTOR('',#5199,10.);
#1506=VECTOR('',#5200,10.);
#1507=VECTOR('',#5201,10.);
#1508=VECTOR('',#5204,10.);
#1509=VECTOR('',#5205,10.);
#1510=VECTOR('',#5206,10.);
#1511=VECTOR('',#5209,10.);
#1512=VECTOR('',#5210,10.);
#1513=VECTOR('',#5213,10.);
#1514=VECTOR('',#5214,10.);
#1515=VECTOR('',#5217,10.);
#1516=VECTOR('',#5236,3.);
#1517=VECTOR('',#5243,10.);
#1518=VECTOR('',#5244,10.);
#1519=VECTOR('',#5245,10.);
#1520=VECTOR('',#5246,10.);
#1521=VECTOR('',#5249,10.);
#1522=VECTOR('',#5250,10.);
#1523=VECTOR('',#5251,10.);
#1524=VECTOR('',#5254,10.);
#1525=VECTOR('',#5255,10.);
#1526=VECTOR('',#5256,10.);
#1527=VECTOR('',#5259,10.);
#1528=VECTOR('',#5260,10.);
#1529=VECTOR('',#5261,10.);
#1530=VECTOR('',#5264,10.);
#1531=VECTOR('',#5265,10.);
#1532=VECTOR('',#5266,10.);
#1533=VECTOR('',#5269,10.);
#1534=VECTOR('',#5270,10.);
#1535=VECTOR('',#5285,5.);
#1536=VECTOR('',#5296,10.);
#1537=VECTOR('',#5299,10.);
#1538=VECTOR('',#5302,10.);
#1539=VECTOR('',#5303,10.);
#1540=VECTOR('',#5304,10.);
#1541=VECTOR('',#5307,10.);
#1542=VECTOR('',#5308,10.);
#1543=VECTOR('',#5309,10.);
#1544=VECTOR('',#5310,10.);
#1545=VECTOR('',#5313,10.);
#1546=VECTOR('',#5314,10.);
#1547=VECTOR('',#5315,10.);
#1548=VECTOR('',#5318,10.);
#1549=VECTOR('',#5319,10.);
#1550=VECTOR('',#5320,10.);
#1551=VECTOR('',#5321,10.);
#1552=VECTOR('',#5346,9.5);
#1553=VECTOR('',#5351,6.5);
#1554=VECTOR('',#5362,1.25);
#1555=VECTOR('',#5369,10.);
#1556=VECTOR('',#5372,10.);
#1557=VECTOR('',#5375,10.);
#1558=VECTOR('',#5376,10.);
#1559=VECTOR('',#5377,10.);
#1560=VECTOR('',#5384,10.);
#1561=VECTOR('',#5391,10.);
#1562=VECTOR('',#5398,10.);
#1563=VECTOR('',#5401,10.);
#1564=VECTOR('',#5402,10.);
#1565=VECTOR('',#5411,10.);
#1566=VECTOR('',#5412,10.);
#1567=VECTOR('',#5413,10.);
#1568=VECTOR('',#5414,10.);
#1569=VECTOR('',#5417,10.);
#1570=VECTOR('',#5418,10.);
#1571=VECTOR('',#5419,10.);
#1572=VECTOR('',#5420,10.);
#1573=VECTOR('',#5441,1.);
#1574=VECTOR('',#5450,1.9);
#1575=VECTOR('',#5467,9.5);
#1576=VECTOR('',#5484,9.5);
#1577=VECTOR('',#5493,6.5);
#1578=VECTOR('',#5506,6.50000009685755);
#1579=VECTOR('',#5511,4.75);
#1580=VECTOR('',#5518,6.5);
#1581=VECTOR('',#5527,8.);
#1582=VECTOR('',#5538,10.);
#1583=VECTOR('',#5539,10.);
#1584=VECTOR('',#5540,10.);
#1585=VECTOR('',#5541,10.);
#1586=VECTOR('',#5544,10.);
#1587=VECTOR('',#5545,10.);
#1588=VECTOR('',#5546,10.);
#1589=VECTOR('',#5549,10.);
#1590=VECTOR('',#5550,10.);
#1591=VECTOR('',#5551,10.);
#1592=VECTOR('',#5554,10.);
#1593=VECTOR('',#5555,10.);
#1594=VECTOR('',#5556,10.);
#1595=VECTOR('',#5559,10.);
#1596=VECTOR('',#5560,10.);
#1597=VECTOR('',#5561,10.);
#1598=VECTOR('',#5564,10.);
#1599=VECTOR('',#5565,10.);
#1600=VECTOR('',#5566,10.);
#1601=VECTOR('',#5569,10.);
#1602=VECTOR('',#5570,10.);
#1603=VECTOR('',#5571,10.);
#1604=VECTOR('',#5574,10.);
#1605=VECTOR('',#5575,10.);
#1606=VERTEX_POINT('',#5609);
#1607=VERTEX_POINT('',#5610);
#1608=VERTEX_POINT('',#5612);
#1609=VERTEX_POINT('',#5614);
#1610=VERTEX_POINT('',#5618);
#1611=VERTEX_POINT('',#5620);
#1612=VERTEX_POINT('',#5624);
#1613=VERTEX_POINT('',#5625);
#1614=VERTEX_POINT('',#5627);
#1615=VERTEX_POINT('',#5629);
#1616=VERTEX_POINT('',#5633);
#1617=VERTEX_POINT('',#5634);
#1618=VERTEX_POINT('',#5636);
#1619=VERTEX_POINT('',#5638);
#1620=VERTEX_POINT('',#5642);
#1621=VERTEX_POINT('',#5644);
#1622=VERTEX_POINT('',#5646);
#1623=VERTEX_POINT('',#5648);
#1624=VERTEX_POINT('',#5653);
#1625=VERTEX_POINT('',#5655);
#1626=VERTEX_POINT('',#5659);
#1627=VERTEX_POINT('',#5662);
#1628=VERTEX_POINT('',#5664);
#1629=VERTEX_POINT('',#5666);
#1630=VERTEX_POINT('',#5673);
#1631=VERTEX_POINT('',#5675);
#1632=VERTEX_POINT('',#5677);
#1633=VERTEX_POINT('',#5679);
#1634=VERTEX_POINT('',#5682);
#1635=VERTEX_POINT('',#5684);
#1636=VERTEX_POINT('',#5687);
#1637=VERTEX_POINT('',#5691);
#1638=VERTEX_POINT('',#5693);
#1639=VERTEX_POINT('',#5695);
#1640=VERTEX_POINT('',#5697);
#1641=VERTEX_POINT('',#5699);
#1642=VERTEX_POINT('',#5701);
#1643=VERTEX_POINT('',#5703);
#1644=VERTEX_POINT('',#5705);
#1645=VERTEX_POINT('',#5709);
#1646=VERTEX_POINT('',#5711);
#1647=VERTEX_POINT('',#5713);
#1648=VERTEX_POINT('',#5715);
#1649=VERTEX_POINT('',#5717);
#1650=VERTEX_POINT('',#5720);
#1651=VERTEX_POINT('',#5722);
#1652=VERTEX_POINT('',#5744);
#1653=VERTEX_POINT('',#5745);
#1654=VERTEX_POINT('',#5751);
#1655=VERTEX_POINT('',#5758);
#1656=VERTEX_POINT('',#5759);
#1657=VERTEX_POINT('',#5783);
#1658=VERTEX_POINT('',#5788);
#1659=VERTEX_POINT('',#5829);
#1660=VERTEX_POINT('',#5833);
#1661=VERTEX_POINT('',#5834);
#1662=VERTEX_POINT('',#5849);
#1663=VERTEX_POINT('',#5854);
#1664=VERTEX_POINT('',#5860);
#1665=VERTEX_POINT('',#5862);
#1666=VERTEX_POINT('',#5867);
#1667=VERTEX_POINT('',#5873);
#1668=VERTEX_POINT('',#5875);
#1669=VERTEX_POINT('',#5877);
#1670=VERTEX_POINT('',#5879);
#1671=VERTEX_POINT('',#5881);
#1672=VERTEX_POINT('',#5885);
#1673=VERTEX_POINT('',#5886);
#1674=VERTEX_POINT('',#5902);
#1675=VERTEX_POINT('',#5906);
#1676=VERTEX_POINT('',#5929);
#1677=VERTEX_POINT('',#5930);
#1678=VERTEX_POINT('',#5932);
#1679=VERTEX_POINT('',#5943);
#1680=VERTEX_POINT('',#5944);
#1681=VERTEX_POINT('',#5968);
#1682=VERTEX_POINT('',#5969);
#1683=VERTEX_POINT('',#6009);
#1684=VERTEX_POINT('',#6016);
#1685=VERTEX_POINT('',#6052);
#1686=VERTEX_POINT('',#6053);
#1687=VERTEX_POINT('',#6077);
#1688=VERTEX_POINT('',#6082);
#1689=VERTEX_POINT('',#6089);
#1690=VERTEX_POINT('',#6090);
#1691=VERTEX_POINT('',#6119);
#1692=VERTEX_POINT('',#6120);
#1693=VERTEX_POINT('',#6132);
#1694=VERTEX_POINT('',#6137);
#1695=VERTEX_POINT('',#6151);
#1696=VERTEX_POINT('',#6153);
#1697=VERTEX_POINT('',#6157);
#1698=VERTEX_POINT('',#6159);
#1699=VERTEX_POINT('',#6200);
#1700=VERTEX_POINT('',#6204);
#1701=VERTEX_POINT('',#6205);
#1702=VERTEX_POINT('',#6207);
#1703=VERTEX_POINT('',#6209);
#1704=VERTEX_POINT('',#6232);
#1705=VERTEX_POINT('',#6237);
#1706=VERTEX_POINT('',#6278);
#1707=VERTEX_POINT('',#6301);
#1708=VERTEX_POINT('',#6302);
#1709=VERTEX_POINT('',#6320);
#1710=VERTEX_POINT('',#6325);
#1711=VERTEX_POINT('',#6343);
#1712=VERTEX_POINT('',#6347);
#1713=VERTEX_POINT('',#6356);
#1714=VERTEX_POINT('',#6383);
#1715=VERTEX_POINT('',#6390);
#1716=VERTEX_POINT('',#6394);
#1717=VERTEX_POINT('',#6396);
#1718=VERTEX_POINT('',#6400);
#1719=VERTEX_POINT('',#6401);
#1720=VERTEX_POINT('',#6403);
#1721=VERTEX_POINT('',#6405);
#1722=VERTEX_POINT('',#6420);
#1723=VERTEX_POINT('',#6421);
#1724=VERTEX_POINT('',#6445);
#1725=VERTEX_POINT('',#6447);
#1726=VERTEX_POINT('',#6449);
#1727=VERTEX_POINT('',#6508);
#1728=VERTEX_POINT('',#6509);
#1729=VERTEX_POINT('',#6533);
#1730=VERTEX_POINT('',#6535);
#1731=VERTEX_POINT('',#6537);
#1732=VERTEX_POINT('',#6601);
#1733=VERTEX_POINT('',#6603);
#1734=VERTEX_POINT('',#6607);
#1735=VERTEX_POINT('',#6622);
#1736=VERTEX_POINT('',#6624);
#1737=VERTEX_POINT('',#6629);
#1738=VERTEX_POINT('',#6633);
#1739=VERTEX_POINT('',#6637);
#1740=VERTEX_POINT('',#6641);
#1741=VERTEX_POINT('',#6645);
#1742=VERTEX_POINT('',#6649);
#1743=VERTEX_POINT('',#6656);
#1744=VERTEX_POINT('',#6659);
#1745=VERTEX_POINT('',#6660);
#1746=VERTEX_POINT('',#6672);
#1747=VERTEX_POINT('',#6676);
#1748=VERTEX_POINT('',#6684);
#1749=VERTEX_POINT('',#6692);
#1750=VERTEX_POINT('',#6694);
#1751=VERTEX_POINT('',#6699);
#1752=VERTEX_POINT('',#6701);
#1753=VERTEX_POINT('',#6714);
#1754=VERTEX_POINT('',#6716);
#1755=VERTEX_POINT('',#6721);
#1756=VERTEX_POINT('',#6723);
#1757=VERTEX_POINT('',#6762);
#1758=VERTEX_POINT('',#6763);
#1759=VERTEX_POINT('',#6771);
#1760=VERTEX_POINT('',#6777);
#1761=VERTEX_POINT('',#6834);
#1762=VERTEX_POINT('',#6835);
#1763=VERTEX_POINT('',#6886);
#1764=VERTEX_POINT('',#6887);
#1765=VERTEX_POINT('',#6933);
#1766=VERTEX_POINT('',#6934);
#1767=VERTEX_POINT('',#7034);
#1768=VERTEX_POINT('',#7035);
#1769=VERTEX_POINT('',#7095);
#1770=VERTEX_POINT('',#7096);
#1771=VERTEX_POINT('',#7147);
#1772=VERTEX_POINT('',#7148);
#1773=VERTEX_POINT('',#7194);
#1774=VERTEX_POINT('',#7195);
#1775=VERTEX_POINT('',#7239);
#1776=VERTEX_POINT('',#7240);
#1777=VERTEX_POINT('',#7291);
#1778=VERTEX_POINT('',#7310);
#1779=VERTEX_POINT('',#7336);
#1780=VERTEX_POINT('',#7337);
#1781=VERTEX_POINT('',#7350);
#1782=VERTEX_POINT('',#7354);
#1783=VERTEX_POINT('',#7356);
#1784=VERTEX_POINT('',#7358);
#1785=VERTEX_POINT('',#7391);
#1786=VERTEX_POINT('',#7392);
#1787=VERTEX_POINT('',#7406);
#1788=VERTEX_POINT('',#7411);
#1789=VERTEX_POINT('',#7458);
#1790=VERTEX_POINT('',#7459);
#1791=VERTEX_POINT('',#7505);
#1792=VERTEX_POINT('',#7506);
#1793=VERTEX_POINT('',#7557);
#1794=VERTEX_POINT('',#7558);
#1795=VERTEX_POINT('',#7646);
#1796=VERTEX_POINT('',#7647);
#1797=VERTEX_POINT('',#7710);
#1798=VERTEX_POINT('',#7711);
#1799=VERTEX_POINT('',#7757);
#1800=VERTEX_POINT('',#7758);
#1801=VERTEX_POINT('',#7809);
#1802=VERTEX_POINT('',#7810);
#1803=VERTEX_POINT('',#7856);
#1804=VERTEX_POINT('',#7857);
#1805=VERTEX_POINT('',#7880);
#1806=VERTEX_POINT('',#7882);
#1807=VERTEX_POINT('',#7899);
#1808=VERTEX_POINT('',#7901);
#1809=VERTEX_POINT('',#7905);
#1810=VERTEX_POINT('',#7907);
#1811=VERTEX_POINT('',#7911);
#1812=VERTEX_POINT('',#7913);
#1813=VERTEX_POINT('',#7917);
#1814=VERTEX_POINT('',#7921);
#1815=VERTEX_POINT('',#7929);
#1816=VERTEX_POINT('',#7931);
#1817=VERTEX_POINT('',#7933);
#1818=VERTEX_POINT('',#7937);
#1819=VERTEX_POINT('',#7939);
#1820=VERTEX_POINT('',#7943);
#1821=VERTEX_POINT('',#7945);
#1822=VERTEX_POINT('',#7949);
#1823=VERTEX_POINT('',#7951);
#1824=VERTEX_POINT('',#7953);
#1825=VERTEX_POINT('',#7955);
#1826=VERTEX_POINT('',#7957);
#1827=VERTEX_POINT('',#7959);
#1828=VERTEX_POINT('',#7963);
#1829=VERTEX_POINT('',#7967);
#1830=VERTEX_POINT('',#7971);
#1831=VERTEX_POINT('',#7975);
#1832=VERTEX_POINT('',#7979);
#1833=VERTEX_POINT('',#7981);
#1834=VERTEX_POINT('',#7984);
#1835=VERTEX_POINT('',#7988);
#1836=VERTEX_POINT('',#7990);
#1837=VERTEX_POINT('',#7995);
#1838=VERTEX_POINT('',#7996);
#1839=VERTEX_POINT('',#7998);
#1840=VERTEX_POINT('',#8000);
#1841=VERTEX_POINT('',#8004);
#1842=VERTEX_POINT('',#8006);
#1843=VERTEX_POINT('',#8010);
#1844=VERTEX_POINT('',#8013);
#1845=VERTEX_POINT('',#8015);
#1846=VERTEX_POINT('',#8019);
#1847=VERTEX_POINT('',#8023);
#1848=VERTEX_POINT('',#8035);
#1849=VERTEX_POINT('',#8037);
#1850=VERTEX_POINT('',#8040);
#1851=VERTEX_POINT('',#8044);
#1852=VERTEX_POINT('',#8048);
#1853=VERTEX_POINT('',#8050);
#1854=VERTEX_POINT('',#8053);
#1855=VERTEX_POINT('',#8057);
#1856=VERTEX_POINT('',#8061);
#1857=VERTEX_POINT('',#8062);
#1858=VERTEX_POINT('',#8064);
#1859=VERTEX_POINT('',#8066);
#1860=VERTEX_POINT('',#8070);
#1861=VERTEX_POINT('',#8072);
#1862=VERTEX_POINT('',#8076);
#1863=VERTEX_POINT('',#8080);
#1864=VERTEX_POINT('',#8088);
#1865=VERTEX_POINT('',#8089);
#1866=VERTEX_POINT('',#8091);
#1867=VERTEX_POINT('',#8096);
#1868=VERTEX_POINT('',#8100);
#1869=VERTEX_POINT('',#8103);
#1870=VERTEX_POINT('',#8104);
#1871=VERTEX_POINT('',#8106);
#1872=VERTEX_POINT('',#8108);
#1873=VERTEX_POINT('',#8112);
#1874=VERTEX_POINT('',#8114);
#1875=VERTEX_POINT('',#8118);
#1876=VERTEX_POINT('',#8120);
#1877=VERTEX_POINT('',#8124);
#1878=VERTEX_POINT('',#8126);
#1879=VERTEX_POINT('',#8130);
#1880=VERTEX_POINT('',#8132);
#1881=VERTEX_POINT('',#8140);
#1882=VERTEX_POINT('',#8142);
#1883=VERTEX_POINT('',#8144);
#1884=VERTEX_POINT('',#8153);
#1885=VERTEX_POINT('',#8154);
#1886=VERTEX_POINT('',#8156);
#1887=VERTEX_POINT('',#8158);
#1888=VERTEX_POINT('',#8162);
#1889=VERTEX_POINT('',#8164);
#1890=VERTEX_POINT('',#8168);
#1891=VERTEX_POINT('',#8169);
#1892=VERTEX_POINT('',#8171);
#1893=VERTEX_POINT('',#8173);
#1894=VERTEX_POINT('',#8177);
#1895=VERTEX_POINT('',#8179);
#1896=VERTEX_POINT('',#8183);
#1897=VERTEX_POINT('',#8184);
#1898=VERTEX_POINT('',#8186);
#1899=VERTEX_POINT('',#8188);
#1900=VERTEX_POINT('',#8195);
#1901=VERTEX_POINT('',#8198);
#1902=VERTEX_POINT('',#8205);
#1903=VERTEX_POINT('',#8209);
#1904=VERTEX_POINT('',#8215);
#1905=VERTEX_POINT('',#8217);
#1906=VERTEX_POINT('',#8221);
#1907=VERTEX_POINT('',#8222);
#1908=VERTEX_POINT('',#8224);
#1909=VERTEX_POINT('',#8226);
#1910=VERTEX_POINT('',#8230);
#1911=VERTEX_POINT('',#8232);
#1912=VERTEX_POINT('',#8236);
#1913=VERTEX_POINT('',#8238);
#1914=VERTEX_POINT('',#8242);
#1915=VERTEX_POINT('',#8244);
#1916=VERTEX_POINT('',#8248);
#1917=VERTEX_POINT('',#8250);
#1918=VERTEX_POINT('',#8260);
#1919=VERTEX_POINT('',#8261);
#1920=VERTEX_POINT('',#8263);
#1921=VERTEX_POINT('',#8265);
#1922=VERTEX_POINT('',#8269);
#1923=VERTEX_POINT('',#8270);
#1924=VERTEX_POINT('',#8272);
#1925=VERTEX_POINT('',#8274);
#1926=VERTEX_POINT('',#8281);
#1927=VERTEX_POINT('',#8287);
#1928=VERTEX_POINT('',#8289);
#1929=VERTEX_POINT('',#8294);
#1930=VERTEX_POINT('',#8300);
#1931=VERTEX_POINT('',#8302);
#1932=VERTEX_POINT('',#8304);
#1933=VERTEX_POINT('',#8308);
#1934=VERTEX_POINT('',#8310);
#1935=VERTEX_POINT('',#8315);
#1936=VERTEX_POINT('',#8316);
#1937=VERTEX_POINT('',#8321);
#1938=VERTEX_POINT('',#8325);
#1939=VERTEX_POINT('',#8328);
#1940=VERTEX_POINT('',#8332);
#1941=VERTEX_POINT('',#8334);
#1942=VERTEX_POINT('',#8337);
#1943=VERTEX_POINT('',#8342);
#1944=VERTEX_POINT('',#8346);
#1945=VERTEX_POINT('',#8348);
#1946=VERTEX_POINT('',#8353);
#1947=VERTEX_POINT('',#8355);
#1948=VERTEX_POINT('',#8362);
#1949=VERTEX_POINT('',#8363);
#1950=VERTEX_POINT('',#8365);
#1951=VERTEX_POINT('',#8367);
#1952=VERTEX_POINT('',#8371);
#1953=VERTEX_POINT('',#8373);
#1954=VERTEX_POINT('',#8377);
#1955=VERTEX_POINT('',#8379);
#1956=VERTEX_POINT('',#8383);
#1957=VERTEX_POINT('',#8385);
#1958=VERTEX_POINT('',#8389);
#1959=VERTEX_POINT('',#8391);
#1960=VERTEX_POINT('',#8395);
#1961=VERTEX_POINT('',#8397);
#1962=VERTEX_POINT('',#8401);
#1963=VERTEX_POINT('',#8403);
#1964=EDGE_CURVE('',#1606,#1607,#1028,.T.);
#1965=EDGE_CURVE('',#1608,#1606,#1029,.T.);
#1966=EDGE_CURVE('',#1609,#1608,#1030,.T.);
#1967=EDGE_CURVE('',#1609,#1607,#1031,.T.);
#1968=EDGE_CURVE('',#1607,#1610,#1032,.T.);
#1969=EDGE_CURVE('',#1611,#1609,#1033,.T.);
#1970=EDGE_CURVE('',#1610,#1611,#1034,.T.);
#1971=EDGE_CURVE('',#1612,#1613,#1035,.T.);
#1972=EDGE_CURVE('',#1614,#1612,#1036,.T.);
#1973=EDGE_CURVE('',#1614,#1615,#1037,.T.);
#1974=EDGE_CURVE('',#1613,#1615,#1038,.T.);
#1975=EDGE_CURVE('',#1616,#1617,#1039,.T.);
#1976=EDGE_CURVE('',#1618,#1616,#1040,.T.);
#1977=EDGE_CURVE('',#1619,#1618,#1041,.T.);
#1978=EDGE_CURVE('',#1619,#1617,#1042,.T.);
#1979=EDGE_CURVE('',#1620,#1606,#1043,.T.);
#1980=EDGE_CURVE('',#1621,#1620,#1044,.T.);
#1981=EDGE_CURVE('',#1622,#1621,#1045,.T.);
#1982=EDGE_CURVE('',#1623,#1622,#1046,.T.);
#1983=EDGE_CURVE('',#1617,#1623,#1047,.T.);
#1984=EDGE_CURVE('',#1608,#1619,#1048,.T.);
#1985=EDGE_CURVE('',#1615,#1624,#1049,.T.);
#1986=EDGE_CURVE('',#1625,#1614,#1050,.T.);
#1987=EDGE_CURVE('',#1625,#1624,#1051,.T.);
#1988=EDGE_CURVE('',#1624,#1626,#1052,.T.);
#1989=EDGE_CURVE('',#1618,#1625,#1053,.T.);
#1990=EDGE_CURVE('',#1627,#1616,#1054,.T.);
#1991=EDGE_CURVE('',#1628,#1627,#1055,.T.);
#1992=EDGE_CURVE('',#1629,#1628,#1056,.T.);
#1993=EDGE_CURVE('',#1629,#1626,#1057,.T.);
#1994=EDGE_CURVE('',#1626,#1620,#1058,.T.);
#1995=EDGE_CURVE('',#1621,#1629,#1059,.T.);
#1996=EDGE_CURVE('',#1628,#1630,#1060,.T.);
#1997=EDGE_CURVE('',#1631,#1630,#1061,.T.);
#1998=EDGE_CURVE('',#1632,#1631,#1062,.T.);
#1999=EDGE_CURVE('',#1633,#1632,#1063,.T.);
#2000=EDGE_CURVE('',#1633,#1622,#1064,.T.);
#2001=EDGE_CURVE('',#1634,#1634,#369,.T.);
#2002=EDGE_CURVE('',#1635,#1635,#370,.T.);
#2003=EDGE_CURVE('',#1627,#1636,#1065,.T.);
#2004=EDGE_CURVE('',#1630,#1636,#1066,.T.);
#2005=EDGE_CURVE('',#1637,#1610,#1067,.T.);
#2006=EDGE_CURVE('',#1638,#1637,#1068,.T.);
#2007=EDGE_CURVE('',#1639,#1638,#371,.T.);
#2008=EDGE_CURVE('',#1640,#1639,#1069,.T.);
#2009=EDGE_CURVE('',#1640,#1641,#1070,.T.);
#2010=EDGE_CURVE('',#1642,#1641,#1071,.T.);
#2011=EDGE_CURVE('',#1643,#1642,#372,.T.);
#2012=EDGE_CURVE('',#1644,#1643,#1072,.T.);
#2013=EDGE_CURVE('',#1613,#1644,#1073,.T.);
#2014=EDGE_CURVE('',#1645,#1611,#1074,.T.);
#2015=EDGE_CURVE('',#1646,#1645,#373,.T.);
#2016=EDGE_CURVE('',#1647,#1646,#374,.T.);
#2017=EDGE_CURVE('',#1648,#1647,#1075,.T.);
#2018=EDGE_CURVE('',#1649,#1648,#375,.T.);
#2019=EDGE_CURVE('',#1637,#1649,#376,.T.);
#2020=EDGE_CURVE('',#1650,#1650,#377,.T.);
#2021=EDGE_CURVE('',#1651,#1651,#378,.T.);
#2022=EDGE_CURVE('',#1652,#1653,#379,.T.);
#2023=EDGE_CURVE('',#1653,#1643,#207,.T.);
#2024=EDGE_CURVE('',#1643,#1654,#380,.T.);
#2025=EDGE_CURVE('',#1654,#1652,#208,.T.);
#2026=EDGE_CURVE('',#1655,#1656,#381,.T.);
#2027=EDGE_CURVE('',#1656,#1653,#382,.T.);
#2028=EDGE_CURVE('',#1652,#1655,#383,.T.);
#2029=EDGE_CURVE('',#1655,#1657,#209,.T.);
#2030=EDGE_CURVE('',#1657,#1658,#384,.T.);
#2031=EDGE_CURVE('',#1658,#1656,#210,.T.);
#2032=EDGE_CURVE('',#1657,#1659,#169,.T.);
#2033=EDGE_CURVE('',#1659,#1658,#170,.T.);
#2034=EDGE_CURVE('',#1660,#1661,#211,.T.);
#2035=EDGE_CURVE('',#1661,#1662,#385,.T.);
#2036=EDGE_CURVE('',#1662,#1641,#386,.T.);
#2037=EDGE_CURVE('',#1641,#1660,#387,.T.);
#2038=EDGE_CURVE('',#1663,#1642,#388,.T.);
#2039=EDGE_CURVE('',#1662,#1663,#1076,.T.);
#2040=EDGE_CURVE('',#1663,#1654,#389,.T.);
#2041=EDGE_CURVE('',#1659,#1664,#1077,.T.);
#2042=EDGE_CURVE('',#1664,#1665,#390,.T.);
#2043=EDGE_CURVE('',#1665,#1658,#1078,.T.);
#2044=EDGE_CURVE('',#1655,#1652,#1079,.T.);
#2045=EDGE_CURVE('',#1666,#1666,#391,.T.);
#2046=EDGE_CURVE('',#1663,#1659,#1080,.T.);
#2047=EDGE_CURVE('',#1661,#1631,#1081,.T.);
#2048=EDGE_CURVE('',#1636,#1667,#1082,.T.);
#2049=EDGE_CURVE('',#1668,#1667,#1083,.T.);
#2050=EDGE_CURVE('',#1669,#1668,#1084,.T.);
#2051=EDGE_CURVE('',#1670,#1669,#1085,.T.);
#2052=EDGE_CURVE('',#1671,#1670,#1086,.T.);
#2053=EDGE_CURVE('',#1671,#1664,#1087,.T.);
#2054=EDGE_CURVE('',#1672,#1673,#212,.T.);
#2055=EDGE_CURVE('',#1673,#1640,#392,.T.);
#2056=EDGE_CURVE('',#1640,#1674,#393,.T.);
#2057=EDGE_CURVE('',#1674,#1672,#394,.T.);
#2058=EDGE_CURVE('',#1639,#1675,#395,.T.);
#2059=EDGE_CURVE('',#1675,#1674,#1088,.T.);
#2060=EDGE_CURVE('',#1676,#1677,#396,.T.);
#2061=EDGE_CURVE('',#1677,#1678,#213,.T.);
#2062=EDGE_CURVE('',#1678,#1638,#397,.T.);
#2063=EDGE_CURVE('',#1638,#1676,#214,.T.);
#2064=EDGE_CURVE('',#1679,#1680,#398,.T.);
#2065=EDGE_CURVE('',#1680,#1677,#399,.T.);
#2066=EDGE_CURVE('',#1676,#1679,#400,.T.);
#2067=EDGE_CURVE('',#1681,#1682,#401,.T.);
#2068=EDGE_CURVE('',#1682,#1680,#215,.T.);
#2069=EDGE_CURVE('',#1679,#1681,#216,.T.);
#2070=EDGE_CURVE('',#1681,#1683,#171,.T.);
#2071=EDGE_CURVE('',#1683,#1682,#172,.T.);
#2072=EDGE_CURVE('',#1678,#1675,#402,.T.);
#2073=EDGE_CURVE('',#1677,#1680,#1089,.T.);
#2074=EDGE_CURVE('',#1684,#1684,#403,.T.);
#2075=EDGE_CURVE('',#1681,#1649,#1090,.T.);
#2076=EDGE_CURVE('',#1648,#1683,#1091,.T.);
#2077=EDGE_CURVE('',#1685,#1686,#404,.T.);
#2078=EDGE_CURVE('',#1686,#1670,#173,.T.);
#2079=EDGE_CURVE('',#1670,#1685,#174,.T.);
#2080=EDGE_CURVE('',#1685,#1687,#217,.T.);
#2081=EDGE_CURVE('',#1687,#1688,#405,.T.);
#2082=EDGE_CURVE('',#1688,#1686,#218,.T.);
#2083=EDGE_CURVE('',#1689,#1690,#406,.T.);
#2084=EDGE_CURVE('',#1690,#1688,#407,.T.);
#2085=EDGE_CURVE('',#1687,#1689,#408,.T.);
#2086=EDGE_CURVE('',#1691,#1692,#219,.T.);
#2087=EDGE_CURVE('',#1692,#1690,#220,.T.);
#2088=EDGE_CURVE('',#1689,#1693,#221,.T.);
#2089=EDGE_CURVE('',#1693,#1694,#222,.T.);
#2090=EDGE_CURVE('',#1694,#1691,#223,.T.);
#2091=EDGE_CURVE('',#1695,#1692,#1092,.T.);
#2092=EDGE_CURVE('',#1695,#1696,#409,.T.);
#2093=EDGE_CURVE('',#1686,#1696,#1093,.T.);
#2094=EDGE_CURVE('',#1697,#1691,#1094,.F.);
#2095=EDGE_CURVE('',#1697,#1698,#224,.T.);
#2096=EDGE_CURVE('',#1698,#1695,#1095,.T.);
#2097=EDGE_CURVE('',#1694,#1697,#225,.T.);
#2098=EDGE_CURVE('',#1693,#1669,#175,.T.);
#2099=EDGE_CURVE('',#1699,#1669,#410,.T.);
#2100=EDGE_CURVE('',#1699,#1698,#176,.T.);
#2101=EDGE_CURVE('',#1700,#1701,#411,.T.);
#2102=EDGE_CURVE('',#1701,#1702,#412,.T.);
#2103=EDGE_CURVE('',#1702,#1703,#413,.T.);
#2104=EDGE_CURVE('',#1703,#1700,#414,.T.);
#2105=EDGE_CURVE('',#1700,#1704,#226,.T.);
#2106=EDGE_CURVE('',#1704,#1705,#415,.T.);
#2107=EDGE_CURVE('',#1705,#1701,#227,.T.);
#2108=EDGE_CURVE('',#1704,#1706,#177,.T.);
#2109=EDGE_CURVE('',#1706,#1705,#178,.T.);
#2110=EDGE_CURVE('',#1707,#1708,#228,.T.);
#2111=EDGE_CURVE('',#1708,#1703,#229,.T.);
#2112=EDGE_CURVE('',#1702,#1709,#230,.T.);
#2113=EDGE_CURVE('',#1709,#1710,#231,.T.);
#2114=EDGE_CURVE('',#1710,#1707,#232,.T.);
#2115=EDGE_CURVE('',#1706,#1647,#1096,.T.);
#2116=EDGE_CURVE('',#1646,#1705,#1097,.T.);
#2117=EDGE_CURVE('',#1700,#1703,#1098,.T.);
#2118=EDGE_CURVE('',#1711,#1708,#179,.T.);
#2119=EDGE_CURVE('',#1711,#1706,#1099,.T.);
#2120=EDGE_CURVE('',#1710,#1712,#1100,.T.);
#2121=EDGE_CURVE('',#1707,#1712,#233,.F.);
#2122=EDGE_CURVE('',#1713,#1713,#416,.T.);
#2123=EDGE_CURVE('',#1712,#1714,#234,.F.);
#2124=EDGE_CURVE('',#1714,#1715,#180,.T.);
#2125=EDGE_CURVE('',#1711,#1715,#417,.T.);
#2126=EDGE_CURVE('',#1715,#1716,#1101,.T.);
#2127=EDGE_CURVE('',#1716,#1717,#418,.T.);
#2128=EDGE_CURVE('',#1717,#1711,#1102,.T.);
#2129=EDGE_CURVE('',#1718,#1719,#419,.T.);
#2130=EDGE_CURVE('',#1719,#1720,#420,.T.);
#2131=EDGE_CURVE('',#1720,#1721,#421,.T.);
#2132=EDGE_CURVE('',#1721,#1718,#235,.T.);
#2133=EDGE_CURVE('',#1722,#1723,#422,.T.);
#2134=EDGE_CURVE('',#1723,#1720,#1103,.T.);
#2135=EDGE_CURVE('',#1719,#1722,#1104,.T.);
#2136=EDGE_CURVE('',#1721,#1724,#181,.T.);
#2137=EDGE_CURVE('',#1724,#1725,#423,.T.);
#2138=EDGE_CURVE('',#1725,#1726,#182,.T.);
#2139=EDGE_CURVE('',#1726,#1718,#236,.T.);
#2140=EDGE_CURVE('',#1727,#1728,#424,.T.);
#2141=EDGE_CURVE('',#1728,#1725,#183,.T.);
#2142=EDGE_CURVE('',#1724,#1727,#184,.T.);
#2143=EDGE_CURVE('',#1729,#1728,#185,.T.);
#2144=EDGE_CURVE('',#1727,#1730,#186,.T.);
#2145=EDGE_CURVE('',#1730,#1731,#237,.T.);
#2146=EDGE_CURVE('',#1731,#1729,#238,.T.);
#2147=EDGE_CURVE('',#1730,#1732,#425,.T.);
#2148=EDGE_CURVE('',#1732,#1733,#426,.T.);
#2149=EDGE_CURVE('',#1733,#1731,#427,.T.);
#2150=EDGE_CURVE('',#1734,#1716,#428,.T.);
#2151=EDGE_CURVE('',#1716,#1733,#1105,.T.);
#2152=EDGE_CURVE('',#1732,#1734,#1106,.T.);
#2153=EDGE_CURVE('',#1668,#1722,#429,.T.);
#2154=EDGE_CURVE('',#1722,#1699,#1107,.T.);
#2155=EDGE_CURVE('',#1668,#1723,#430,.T.);
#2156=EDGE_CURVE('',#1734,#1717,#431,.T.);
#2157=EDGE_CURVE('',#1645,#1709,#1108,.T.);
#2158=EDGE_CURVE('',#1683,#1675,#1109,.T.);
#2159=EDGE_CURVE('',#1735,#1717,#1110,.T.);
#2160=EDGE_CURVE('',#1735,#1736,#1111,.T.);
#2161=EDGE_CURVE('',#1736,#1633,#1112,.T.);
#2162=EDGE_CURVE('',#1632,#1672,#1113,.T.);
#2163=EDGE_CURVE('',#1734,#1737,#1114,.T.);
#2164=EDGE_CURVE('',#1737,#1735,#187,.T.);
#2165=EDGE_CURVE('',#1738,#1732,#1115,.T.);
#2166=EDGE_CURVE('',#1737,#1738,#1116,.T.);
#2167=EDGE_CURVE('',#1739,#1727,#1117,.T.);
#2168=EDGE_CURVE('',#1738,#1739,#188,.T.);
#2169=EDGE_CURVE('',#1740,#1724,#1118,.T.);
#2170=EDGE_CURVE('',#1739,#1740,#189,.T.);
#2171=EDGE_CURVE('',#1741,#1720,#1119,.T.);
#2172=EDGE_CURVE('',#1740,#1741,#190,.T.);
#2173=EDGE_CURVE('',#1742,#1723,#1120,.T.);
#2174=EDGE_CURVE('',#1741,#1742,#1121,.T.);
#2175=EDGE_CURVE('',#1667,#1742,#191,.T.);
#2176=EDGE_CURVE('',#1736,#1623,#1122,.T.);
#2177=EDGE_CURVE('',#1743,#1743,#432,.T.);
#2178=EDGE_CURVE('',#1744,#1745,#192,.T.);
#2179=EDGE_CURVE('',#1745,#1744,#433,.T.);
#2180=EDGE_CURVE('',#1745,#1743,#1123,.T.);
#2181=EDGE_CURVE('',#1729,#1745,#1124,.T.);
#2182=EDGE_CURVE('',#1744,#1726,#1125,.T.);
#2183=EDGE_CURVE('',#1696,#1671,#434,.T.);
#2184=EDGE_CURVE('',#1689,#1687,#1126,.T.);
#2185=EDGE_CURVE('',#1746,#1746,#435,.T.);
#2186=EDGE_CURVE('',#1666,#1747,#1127,.T.);
#2187=EDGE_CURVE('',#1747,#1747,#436,.T.);
#2188=EDGE_CURVE('',#1665,#1644,#437,.T.);
#2189=EDGE_CURVE('',#1684,#1650,#1128,.T.);
#2190=EDGE_CURVE('',#1746,#1748,#1129,.T.);
#2191=EDGE_CURVE('',#1748,#1748,#438,.T.);
#2192=EDGE_CURVE('',#1713,#1651,#1130,.T.);
#2193=EDGE_CURVE('',#1645,#1714,#1131,.T.);
#2194=EDGE_CURVE('',#1749,#1749,#439,.T.);
#2195=EDGE_CURVE('',#1749,#1750,#1132,.T.);
#2196=EDGE_CURVE('',#1635,#1749,#1133,.T.);
#2197=EDGE_CURVE('',#1751,#1751,#440,.T.);
#2198=EDGE_CURVE('',#1751,#1752,#1134,.T.);
#2199=EDGE_CURVE('',#1634,#1751,#1135,.T.);
#2200=EDGE_CURVE('',#1673,#1660,#1136,.T.);
#2201=EDGE_CURVE('',#1612,#1695,#1137,.T.);
#2202=EDGE_CURVE('',#1753,#1753,#441,.T.);
#2203=EDGE_CURVE('',#1753,#1754,#1138,.T.);
#2204=EDGE_CURVE('',#1754,#1754,#442,.T.);
#2205=EDGE_CURVE('',#1755,#1755,#443,.T.);
#2206=EDGE_CURVE('',#1755,#1756,#1139,.T.);
#2207=EDGE_CURVE('',#1756,#1756,#444,.T.);
#2208=EDGE_CURVE('',#1757,#1758,#239,.T.);
#2209=EDGE_CURVE('',#1758,#1759,#240,.T.);
#2210=EDGE_CURVE('',#1759,#1760,#241,.T.);
#2211=EDGE_CURVE('',#1760,#1757,#242,.T.);
#2212=EDGE_CURVE('',#1761,#1762,#243,.T.);
#2213=EDGE_CURVE('',#1762,#1758,#244,.T.);
#2214=EDGE_CURVE('',#1757,#1761,#245,.T.);
#2215=EDGE_CURVE('',#1763,#1764,#246,.T.);
#2216=EDGE_CURVE('',#1764,#1762,#247,.T.);
#2217=EDGE_CURVE('',#1761,#1763,#248,.T.);
#2218=EDGE_CURVE('',#1765,#1766,#249,.T.);
#2219=EDGE_CURVE('',#1766,#1764,#250,.T.);
#2220=EDGE_CURVE('',#1763,#1765,#251,.T.);
#2221=EDGE_CURVE('',#1767,#1768,#252,.T.);
#2222=EDGE_CURVE('',#1768,#1766,#253,.T.);
#2223=EDGE_CURVE('',#1765,#1767,#254,.T.);
#2224=EDGE_CURVE('',#1769,#1770,#255,.T.);
#2225=EDGE_CURVE('',#1770,#1768,#256,.T.);
#2226=EDGE_CURVE('',#1767,#1769,#257,.T.);
#2227=EDGE_CURVE('',#1771,#1772,#258,.T.);
#2228=EDGE_CURVE('',#1772,#1770,#259,.T.);
#2229=EDGE_CURVE('',#1769,#1771,#260,.T.);
#2230=EDGE_CURVE('',#1773,#1774,#261,.T.);
#2231=EDGE_CURVE('',#1774,#1772,#262,.T.);
#2232=EDGE_CURVE('',#1771,#1773,#263,.T.);
#2233=EDGE_CURVE('',#1775,#1776,#264,.T.);
#2234=EDGE_CURVE('',#1776,#1774,#265,.T.);
#2235=EDGE_CURVE('',#1773,#1775,#266,.T.);
#2236=EDGE_CURVE('',#1775,#1777,#267,.T.);
#2237=EDGE_CURVE('',#1777,#1778,#268,.T.);
#2238=EDGE_CURVE('',#1778,#1776,#269,.T.);
#2239=EDGE_CURVE('',#1779,#1780,#1140,.T.);
#2240=EDGE_CURVE('',#1779,#1778,#270,.T.);
#2241=EDGE_CURVE('',#1777,#1780,#271,.T.);
#2242=EDGE_CURVE('',#1781,#1767,#1141,.T.);
#2243=EDGE_CURVE('',#1781,#1775,#1142,.T.);
#2244=EDGE_CURVE('',#1765,#1782,#1143,.T.);
#2245=EDGE_CURVE('',#1782,#1783,#445,.T.);
#2246=EDGE_CURVE('',#1783,#1784,#1144,.T.);
#2247=EDGE_CURVE('',#1784,#1781,#446,.T.);
#2248=EDGE_CURVE('',#1760,#1782,#1145,.T.);
#2249=EDGE_CURVE('',#1785,#1786,#272,.T.);
#2250=EDGE_CURVE('',#1786,#1787,#273,.T.);
#2251=EDGE_CURVE('',#1787,#1788,#274,.T.);
#2252=EDGE_CURVE('',#1788,#1785,#275,.T.);
#2253=EDGE_CURVE('',#1789,#1790,#276,.T.);
#2254=EDGE_CURVE('',#1790,#1788,#277,.T.);
#2255=EDGE_CURVE('',#1787,#1789,#278,.T.);
#2256=EDGE_CURVE('',#1791,#1792,#279,.T.);
#2257=EDGE_CURVE('',#1792,#1790,#280,.T.);
#2258=EDGE_CURVE('',#1789,#1791,#281,.T.);
#2259=EDGE_CURVE('',#1793,#1794,#282,.T.);
#2260=EDGE_CURVE('',#1794,#1792,#283,.T.);
#2261=EDGE_CURVE('',#1791,#1793,#284,.T.);
#2262=EDGE_CURVE('',#1795,#1796,#285,.T.);
#2263=EDGE_CURVE('',#1796,#1794,#286,.T.);
#2264=EDGE_CURVE('',#1793,#1795,#287,.T.);
#2265=EDGE_CURVE('',#1797,#1798,#288,.T.);
#2266=EDGE_CURVE('',#1798,#1796,#289,.T.);
#2267=EDGE_CURVE('',#1795,#1797,#290,.T.);
#2268=EDGE_CURVE('',#1799,#1800,#291,.T.);
#2269=EDGE_CURVE('',#1800,#1798,#292,.T.);
#2270=EDGE_CURVE('',#1797,#1799,#293,.T.);
#2271=EDGE_CURVE('',#1801,#1802,#294,.T.);
#2272=EDGE_CURVE('',#1802,#1800,#295,.T.);
#2273=EDGE_CURVE('',#1799,#1801,#296,.T.);
#2274=EDGE_CURVE('',#1803,#1804,#297,.T.);
#2275=EDGE_CURVE('',#1804,#1802,#298,.T.);
#2276=EDGE_CURVE('',#1801,#1803,#299,.T.);
#2277=EDGE_CURVE('',#1780,#1805,#1146,.T.);
#2278=EDGE_CURVE('',#1805,#1806,#447,.T.);
#2279=EDGE_CURVE('',#1803,#1806,#1147,.T.);
#2280=EDGE_CURVE('',#1801,#1778,#1148,.T.);
#2281=EDGE_CURVE('',#1799,#1774,#1149,.T.);
#2282=EDGE_CURVE('',#1797,#1772,#1150,.T.);
#2283=EDGE_CURVE('',#1795,#1770,#1151,.T.);
#2284=EDGE_CURVE('',#1793,#1764,#1152,.T.);
#2285=EDGE_CURVE('',#1791,#1762,#1153,.T.);
#2286=EDGE_CURVE('',#1789,#1758,#1154,.T.);
#2287=EDGE_CURVE('',#1787,#1807,#1155,.T.);
#2288=EDGE_CURVE('',#1807,#1808,#448,.T.);
#2289=EDGE_CURVE('',#1808,#1759,#1156,.T.);
#2290=EDGE_CURVE('',#1786,#1809,#1157,.T.);
#2291=EDGE_CURVE('',#1809,#1810,#449,.T.);
#2292=EDGE_CURVE('',#1810,#1807,#1158,.T.);
#2293=EDGE_CURVE('',#1811,#1785,#1159,.T.);
#2294=EDGE_CURVE('',#1811,#1812,#1160,.T.);
#2295=EDGE_CURVE('',#1812,#1809,#1161,.T.);
#2296=EDGE_CURVE('',#1813,#1784,#1162,.T.);
#2297=EDGE_CURVE('',#1813,#1805,#1163,.T.);
#2298=EDGE_CURVE('',#1814,#1783,#1164,.T.);
#2299=EDGE_CURVE('',#1813,#1814,#1165,.T.);
#2300=EDGE_CURVE('',#1814,#1808,#1166,.T.);
#2301=EDGE_CURVE('',#1810,#1805,#1167,.T.);
#2302=EDGE_CURVE('',#1815,#1812,#450,.T.);
#2303=EDGE_CURVE('',#1815,#1816,#1168,.T.);
#2304=EDGE_CURVE('',#1817,#1816,#451,.T.);
#2305=EDGE_CURVE('',#1806,#1817,#1169,.T.);
#2306=EDGE_CURVE('',#1818,#1815,#1170,.T.);
#2307=EDGE_CURVE('',#1818,#1819,#1171,.T.);
#2308=EDGE_CURVE('',#1816,#1819,#1172,.T.);
#2309=EDGE_CURVE('',#1820,#1818,#452,.T.);
#2310=EDGE_CURVE('',#1820,#1821,#1173,.T.);
#2311=EDGE_CURVE('',#1819,#1821,#453,.T.);
#2312=EDGE_CURVE('',#1822,#1820,#1174,.T.);
#2313=EDGE_CURVE('',#1823,#1822,#1175,.T.);
#2314=EDGE_CURVE('',#1824,#1823,#1176,.T.);
#2315=EDGE_CURVE('',#1824,#1825,#1177,.T.);
#2316=EDGE_CURVE('',#1826,#1825,#1178,.T.);
#2317=EDGE_CURVE('',#1827,#1826,#1179,.T.);
#2318=EDGE_CURVE('',#1821,#1827,#1180,.T.);
#2319=EDGE_CURVE('',#1828,#1817,#1181,.T.);
#2320=EDGE_CURVE('',#1828,#1804,#1182,.T.);
#2321=EDGE_CURVE('',#1829,#1827,#1183,.T.);
#2322=EDGE_CURVE('',#1829,#1828,#1184,.T.);
#2323=EDGE_CURVE('',#1830,#1826,#1185,.T.);
#2324=EDGE_CURVE('',#1830,#1829,#1186,.T.);
#2325=EDGE_CURVE('',#1831,#1825,#1187,.T.);
#2326=EDGE_CURVE('',#1831,#1830,#1188,.T.);
#2327=EDGE_CURVE('',#1832,#1832,#454,.T.);
#2328=EDGE_CURVE('',#1832,#1833,#1189,.T.);
#2329=EDGE_CURVE('',#1834,#1834,#455,.T.);
#2330=EDGE_CURVE('',#1834,#1832,#1190,.T.);
#2331=EDGE_CURVE('',#1835,#1835,#456,.T.);
#2332=EDGE_CURVE('',#1835,#1836,#1191,.T.);
#2333=EDGE_CURVE('',#1836,#1836,#457,.T.);
#2334=EDGE_CURVE('',#1837,#1838,#1192,.T.);
#2335=EDGE_CURVE('',#1837,#1839,#1193,.T.);
#2336=EDGE_CURVE('',#1840,#1839,#1194,.T.);
#2337=EDGE_CURVE('',#1838,#1840,#1195,.T.);
#2338=EDGE_CURVE('',#1838,#1841,#1196,.T.);
#2339=EDGE_CURVE('',#1842,#1840,#1197,.T.);
#2340=EDGE_CURVE('',#1841,#1842,#1198,.T.);
#2341=EDGE_CURVE('',#1843,#1824,#1199,.T.);
#2342=EDGE_CURVE('',#1841,#1843,#1200,.T.);
#2343=EDGE_CURVE('',#1844,#1842,#1201,.T.);
#2344=EDGE_CURVE('',#1845,#1844,#1202,.T.);
#2345=EDGE_CURVE('',#1845,#1831,#1203,.T.);
#2346=EDGE_CURVE('',#1846,#1823,#1204,.T.);
#2347=EDGE_CURVE('',#1843,#1846,#1205,.T.);
#2348=EDGE_CURVE('',#1847,#1822,#1206,.T.);
#2349=EDGE_CURVE('',#1846,#1847,#1207,.T.);
#2350=EDGE_CURVE('',#1847,#1811,#1208,.T.);
#2351=EDGE_CURVE('',#1837,#1845,#1209,.T.);
#2352=EDGE_CURVE('',#1839,#1844,#1210,.T.);
#2353=EDGE_CURVE('',#1848,#1848,#458,.T.);
#2354=EDGE_CURVE('',#1849,#1849,#459,.T.);
#2355=EDGE_CURVE('',#1850,#1850,#460,.T.);
#2356=EDGE_CURVE('',#1850,#1848,#1211,.T.);
#2357=EDGE_CURVE('',#1849,#1851,#1212,.T.);
#2358=EDGE_CURVE('',#1851,#1851,#461,.T.);
#2359=EDGE_CURVE('',#1852,#1852,#462,.T.);
#2360=EDGE_CURVE('',#1853,#1853,#463,.T.);
#2361=EDGE_CURVE('',#1854,#1854,#464,.T.);
#2362=EDGE_CURVE('',#1854,#1852,#1213,.T.);
#2363=EDGE_CURVE('',#1853,#1855,#1214,.T.);
#2364=EDGE_CURVE('',#1855,#1855,#465,.T.);
#2365=EDGE_CURVE('',#1856,#1857,#1215,.T.);
#2366=EDGE_CURVE('',#1857,#1858,#1216,.T.);
#2367=EDGE_CURVE('',#1858,#1859,#1217,.T.);
#2368=EDGE_CURVE('',#1859,#1856,#1218,.T.);
#2369=EDGE_CURVE('',#1857,#1860,#1219,.T.);
#2370=EDGE_CURVE('',#1861,#1860,#1220,.T.);
#2371=EDGE_CURVE('',#1858,#1861,#1221,.T.);
#2372=EDGE_CURVE('',#1862,#1861,#1222,.T.);
#2373=EDGE_CURVE('',#1859,#1862,#1223,.T.);
#2374=EDGE_CURVE('',#1863,#1862,#1224,.T.);
#2375=EDGE_CURVE('',#1856,#1863,#1225,.T.);
#2376=EDGE_CURVE('',#1860,#1863,#1226,.T.);
#2377=EDGE_CURVE('',#1864,#1865,#466,.T.);
#2378=EDGE_CURVE('',#1865,#1866,#467,.T.);
#2379=EDGE_CURVE('',#1866,#1866,#468,.T.);
#2380=EDGE_CURVE('',#1865,#1864,#469,.T.);
#2381=EDGE_CURVE('',#1867,#1867,#470,.T.);
#2382=EDGE_CURVE('',#1867,#1864,#1227,.T.);
#2383=EDGE_CURVE('',#1868,#1868,#471,.T.);
#2384=EDGE_CURVE('',#1869,#1870,#1228,.T.);
#2385=EDGE_CURVE('',#1869,#1871,#1229,.T.);
#2386=EDGE_CURVE('',#1871,#1872,#1230,.T.);
#2387=EDGE_CURVE('',#1870,#1872,#1231,.T.);
#2388=EDGE_CURVE('',#1873,#1869,#1232,.T.);
#2389=EDGE_CURVE('',#1873,#1874,#1233,.T.);
#2390=EDGE_CURVE('',#1874,#1871,#1234,.T.);
#2391=EDGE_CURVE('',#1875,#1873,#1235,.T.);
#2392=EDGE_CURVE('',#1875,#1876,#1236,.T.);
#2393=EDGE_CURVE('',#1876,#1874,#1237,.T.);
#2394=EDGE_CURVE('',#1877,#1875,#1238,.T.);
#2395=EDGE_CURVE('',#1877,#1878,#1239,.T.);
#2396=EDGE_CURVE('',#1878,#1876,#1240,.T.);
#2397=EDGE_CURVE('',#1879,#1877,#1241,.T.);
#2398=EDGE_CURVE('',#1879,#1880,#1242,.T.);
#2399=EDGE_CURVE('',#1880,#1878,#1243,.T.);
#2400=EDGE_CURVE('',#1870,#1879,#1244,.T.);
#2401=EDGE_CURVE('',#1872,#1880,#1245,.T.);
#2402=EDGE_CURVE('',#1881,#1881,#472,.T.);
#2403=EDGE_CURVE('',#1881,#1882,#473,.T.);
#2404=EDGE_CURVE('',#1882,#1883,#474,.T.);
#2405=EDGE_CURVE('',#1883,#1882,#475,.T.);
#2406=EDGE_CURVE('',#1883,#1868,#1246,.T.);
#2407=EDGE_CURVE('',#1884,#1885,#476,.T.);
#2408=EDGE_CURVE('',#1884,#1886,#1247,.T.);
#2409=EDGE_CURVE('',#1887,#1886,#477,.T.);
#2410=EDGE_CURVE('',#1885,#1887,#1248,.T.);
#2411=EDGE_CURVE('',#1888,#1884,#1249,.T.);
#2412=EDGE_CURVE('',#1889,#1888,#1250,.T.);
#2413=EDGE_CURVE('',#1886,#1889,#1251,.T.);
#2414=EDGE_CURVE('',#1890,#1891,#1252,.T.);
#2415=EDGE_CURVE('',#1892,#1890,#1253,.T.);
#2416=EDGE_CURVE('',#1893,#1892,#1254,.T.);
#2417=EDGE_CURVE('',#1891,#1893,#1255,.T.);
#2418=EDGE_CURVE('',#1885,#1894,#1256,.T.);
#2419=EDGE_CURVE('',#1895,#1887,#1257,.T.);
#2420=EDGE_CURVE('',#1894,#1895,#1258,.T.);
#2421=EDGE_CURVE('',#1896,#1897,#1259,.T.);
#2422=EDGE_CURVE('',#1898,#1896,#1260,.T.);
#2423=EDGE_CURVE('',#1899,#1898,#1261,.T.);
#2424=EDGE_CURVE('',#1899,#1897,#1262,.T.);
#2425=EDGE_CURVE('',#1897,#1890,#478,.T.);
#2426=EDGE_CURVE('',#1892,#1899,#479,.T.);
#2427=EDGE_CURVE('',#1896,#1900,#480,.T.);
#2428=EDGE_CURVE('',#1900,#1894,#481,.T.);
#2429=EDGE_CURVE('',#1895,#1901,#482,.T.);
#2430=EDGE_CURVE('',#1901,#1898,#483,.T.);
#2431=EDGE_CURVE('',#1893,#1889,#484,.T.);
#2432=EDGE_CURVE('',#1888,#1891,#485,.T.);
#2433=EDGE_CURVE('',#1901,#1902,#1263,.T.);
#2434=EDGE_CURVE('',#1902,#1902,#486,.T.);
#2435=EDGE_CURVE('',#1900,#1903,#1264,.T.);
#2436=EDGE_CURVE('',#1903,#1903,#487,.T.);
#2437=EDGE_CURVE('',#1904,#1904,#488,.T.);
#2438=EDGE_CURVE('',#1904,#1905,#1265,.T.);
#2439=EDGE_CURVE('',#1905,#1905,#489,.T.);
#2440=EDGE_CURVE('',#1906,#1907,#490,.T.);
#2441=EDGE_CURVE('',#1906,#1908,#1266,.T.);
#2442=EDGE_CURVE('',#1909,#1908,#491,.T.);
#2443=EDGE_CURVE('',#1907,#1909,#1267,.T.);
#2444=EDGE_CURVE('',#1907,#1910,#1268,.T.);
#2445=EDGE_CURVE('',#1911,#1909,#1269,.T.);
#2446=EDGE_CURVE('',#1910,#1911,#1270,.T.);
#2447=EDGE_CURVE('',#1912,#1910,#492,.T.);
#2448=EDGE_CURVE('',#1913,#1911,#493,.T.);
#2449=EDGE_CURVE('',#1912,#1913,#1271,.T.);
#2450=EDGE_CURVE('',#1914,#1912,#494,.T.);
#2451=EDGE_CURVE('',#1915,#1913,#495,.T.);
#2452=EDGE_CURVE('',#1914,#1915,#1272,.T.);
#2453=EDGE_CURVE('',#1916,#1914,#496,.T.);
#2454=EDGE_CURVE('',#1917,#1915,#497,.T.);
#2455=EDGE_CURVE('',#1916,#1917,#1273,.T.);
#2456=EDGE_CURVE('',#1906,#1916,#1274,.T.);
#2457=EDGE_CURVE('',#1908,#1917,#1275,.T.);
#2458=EDGE_CURVE('',#1918,#1919,#1276,.T.);
#2459=EDGE_CURVE('',#1920,#1918,#1277,.T.);
#2460=EDGE_CURVE('',#1920,#1921,#1278,.T.);
#2461=EDGE_CURVE('',#1919,#1921,#1279,.T.);
#2462=EDGE_CURVE('',#1922,#1923,#1280,.T.);
#2463=EDGE_CURVE('',#1924,#1922,#1281,.T.);
#2464=EDGE_CURVE('',#1924,#1925,#1282,.T.);
#2465=EDGE_CURVE('',#1923,#1925,#1283,.T.);
#2466=EDGE_CURVE('',#1921,#1924,#498,.T.);
#2467=EDGE_CURVE('',#1925,#1920,#499,.T.);
#2468=EDGE_CURVE('',#1926,#1923,#500,.T.);
#2469=EDGE_CURVE('',#1922,#1926,#501,.T.);
#2470=EDGE_CURVE('',#1918,#1919,#502,.T.);
#2471=EDGE_CURVE('',#1927,#1927,#503,.T.);
#2472=EDGE_CURVE('',#1927,#1928,#1284,.T.);
#2473=EDGE_CURVE('',#1928,#1928,#504,.T.);
#2474=EDGE_CURVE('',#1929,#1929,#505,.T.);
#2475=EDGE_CURVE('',#1929,#1926,#1285,.T.);
#2476=EDGE_CURVE('',#1930,#1930,#506,.T.);
#2477=EDGE_CURVE('',#1930,#1931,#507,.T.);
#2478=EDGE_CURVE('',#1931,#1932,#508,.T.);
#2479=EDGE_CURVE('',#1932,#1931,#509,.T.);
#2480=EDGE_CURVE('',#1932,#1933,#1286,.T.);
#2481=EDGE_CURVE('',#1933,#1934,#510,.T.);
#2482=EDGE_CURVE('',#1934,#1933,#511,.T.);
#2483=EDGE_CURVE('',#1935,#1936,#512,.T.);
#2484=EDGE_CURVE('',#1936,#1935,#513,.T.);
#2485=EDGE_CURVE('',#1936,#1934,#514,.T.);
#2486=EDGE_CURVE('',#1935,#1937,#1287,.T.);
#2487=EDGE_CURVE('',#1937,#1937,#515,.T.);
#2488=EDGE_CURVE('',#1938,#1938,#516,.T.);
#2489=EDGE_CURVE('',#1938,#1939,#1288,.T.);
#2490=EDGE_CURVE('',#1939,#1939,#517,.T.);
#2491=EDGE_CURVE('',#1940,#1940,#518,.T.);
#2492=EDGE_CURVE('',#1941,#1941,#519,.T.);
#2493=EDGE_CURVE('',#1942,#1942,#520,.T.);
#2494=EDGE_CURVE('',#1942,#1940,#1289,.T.);
#2495=EDGE_CURVE('',#1941,#1943,#1290,.T.);
#2496=EDGE_CURVE('',#1943,#1943,#521,.T.);
#2497=EDGE_CURVE('',#1944,#1944,#522,.T.);
#2498=EDGE_CURVE('',#1944,#1945,#1291,.T.);
#2499=EDGE_CURVE('',#1945,#1945,#523,.T.);
#2500=EDGE_CURVE('',#1946,#1946,#524,.T.);
#2501=EDGE_CURVE('',#1946,#1947,#1292,.T.);
#2502=EDGE_CURVE('',#1947,#1947,#525,.T.);
#2503=EDGE_CURVE('',#1948,#1949,#1293,.T.);
#2504=EDGE_CURVE('',#1948,#1950,#1294,.T.);
#2505=EDGE_CURVE('',#1951,#1950,#1295,.T.);
#2506=EDGE_CURVE('',#1949,#1951,#1296,.T.);
#2507=EDGE_CURVE('',#1952,#1949,#1297,.T.);
#2508=EDGE_CURVE('',#1953,#1951,#1298,.T.);
#2509=EDGE_CURVE('',#1952,#1953,#1299,.T.);
#2510=EDGE_CURVE('',#1954,#1952,#1300,.T.);
#2511=EDGE_CURVE('',#1955,#1953,#1301,.T.);
#2512=EDGE_CURVE('',#1954,#1955,#1302,.T.);
#2513=EDGE_CURVE('',#1956,#1954,#1303,.T.);
#2514=EDGE_CURVE('',#1957,#1955,#1304,.T.);
#2515=EDGE_CURVE('',#1956,#1957,#1305,.T.);
#2516=EDGE_CURVE('',#1958,#1956,#1306,.T.);
#2517=EDGE_CURVE('',#1959,#1957,#1307,.T.);
#2518=EDGE_CURVE('',#1958,#1959,#1308,.T.);
#2519=EDGE_CURVE('',#1960,#1958,#1309,.T.);
#2520=EDGE_CURVE('',#1961,#1959,#1310,.T.);
#2521=EDGE_CURVE('',#1960,#1961,#1311,.T.);
#2522=EDGE_CURVE('',#1962,#1960,#1312,.T.);
#2523=EDGE_CURVE('',#1963,#1961,#1313,.T.);
#2524=EDGE_CURVE('',#1962,#1963,#1314,.T.);
#2525=EDGE_CURVE('',#1948,#1962,#1315,.T.);
#2526=EDGE_CURVE('',#1950,#1963,#1316,.T.);
#2527=ORIENTED_EDGE('',*,*,#1964,.F.);
#2528=ORIENTED_EDGE('',*,*,#1965,.F.);
#2529=ORIENTED_EDGE('',*,*,#1966,.F.);
#2530=ORIENTED_EDGE('',*,*,#1967,.T.);
#2531=ORIENTED_EDGE('',*,*,#1968,.F.);
#2532=ORIENTED_EDGE('',*,*,#1967,.F.);
#2533=ORIENTED_EDGE('',*,*,#1969,.F.);
#2534=ORIENTED_EDGE('',*,*,#1970,.F.);
#2535=ORIENTED_EDGE('',*,*,#1971,.F.);
#2536=ORIENTED_EDGE('',*,*,#1972,.F.);
#2537=ORIENTED_EDGE('',*,*,#1973,.T.);
#2538=ORIENTED_EDGE('',*,*,#1974,.F.);
#2539=ORIENTED_EDGE('',*,*,#1975,.F.);
#2540=ORIENTED_EDGE('',*,*,#1976,.F.);
#2541=ORIENTED_EDGE('',*,*,#1977,.F.);
#2542=ORIENTED_EDGE('',*,*,#1978,.T.);
#2543=ORIENTED_EDGE('',*,*,#1979,.F.);
#2544=ORIENTED_EDGE('',*,*,#1980,.F.);
#2545=ORIENTED_EDGE('',*,*,#1981,.F.);
#2546=ORIENTED_EDGE('',*,*,#1982,.F.);
#2547=ORIENTED_EDGE('',*,*,#1983,.F.);
#2548=ORIENTED_EDGE('',*,*,#1978,.F.);
#2549=ORIENTED_EDGE('',*,*,#1984,.F.);
#2550=ORIENTED_EDGE('',*,*,#1965,.T.);
#2551=ORIENTED_EDGE('',*,*,#1985,.F.);
#2552=ORIENTED_EDGE('',*,*,#1973,.F.);
#2553=ORIENTED_EDGE('',*,*,#1986,.F.);
#2554=ORIENTED_EDGE('',*,*,#1987,.T.);
#2555=ORIENTED_EDGE('',*,*,#1988,.F.);
#2556=ORIENTED_EDGE('',*,*,#1987,.F.);
#2557=ORIENTED_EDGE('',*,*,#1989,.F.);
#2558=ORIENTED_EDGE('',*,*,#1976,.T.);
#2559=ORIENTED_EDGE('',*,*,#1990,.F.);
#2560=ORIENTED_EDGE('',*,*,#1991,.F.);
#2561=ORIENTED_EDGE('',*,*,#1992,.F.);
#2562=ORIENTED_EDGE('',*,*,#1993,.T.);
#2563=ORIENTED_EDGE('',*,*,#1994,.F.);
#2564=ORIENTED_EDGE('',*,*,#1993,.F.);
#2565=ORIENTED_EDGE('',*,*,#1995,.F.);
#2566=ORIENTED_EDGE('',*,*,#1980,.T.);
#2567=ORIENTED_EDGE('',*,*,#1981,.T.);
#2568=ORIENTED_EDGE('',*,*,#1995,.T.);
#2569=ORIENTED_EDGE('',*,*,#1992,.T.);
#2570=ORIENTED_EDGE('',*,*,#1996,.T.);
#2571=ORIENTED_EDGE('',*,*,#1997,.F.);
#2572=ORIENTED_EDGE('',*,*,#1998,.F.);
#2573=ORIENTED_EDGE('',*,*,#1999,.F.);
#2574=ORIENTED_EDGE('',*,*,#2000,.T.);
#2575=ORIENTED_EDGE('',*,*,#2001,.T.);
#2576=ORIENTED_EDGE('',*,*,#2002,.T.);
#2577=ORIENTED_EDGE('',*,*,#1991,.T.);
#2578=ORIENTED_EDGE('',*,*,#2003,.T.);
#2579=ORIENTED_EDGE('',*,*,#2004,.F.);
#2580=ORIENTED_EDGE('',*,*,#1996,.F.);
#2581=ORIENTED_EDGE('',*,*,#1974,.T.);
#2582=ORIENTED_EDGE('',*,*,#1985,.T.);
#2583=ORIENTED_EDGE('',*,*,#1988,.T.);
#2584=ORIENTED_EDGE('',*,*,#1994,.T.);
#2585=ORIENTED_EDGE('',*,*,#1979,.T.);
#2586=ORIENTED_EDGE('',*,*,#1964,.T.);
#2587=ORIENTED_EDGE('',*,*,#1968,.T.);
#2588=ORIENTED_EDGE('',*,*,#2005,.F.);
#2589=ORIENTED_EDGE('',*,*,#2006,.F.);
#2590=ORIENTED_EDGE('',*,*,#2007,.F.);
#2591=ORIENTED_EDGE('',*,*,#2008,.F.);
#2592=ORIENTED_EDGE('',*,*,#2009,.T.);
#2593=ORIENTED_EDGE('',*,*,#2010,.F.);
#2594=ORIENTED_EDGE('',*,*,#2011,.F.);
#2595=ORIENTED_EDGE('',*,*,#2012,.F.);
#2596=ORIENTED_EDGE('',*,*,#2013,.F.);
#2597=ORIENTED_EDGE('',*,*,#1970,.T.);
#2598=ORIENTED_EDGE('',*,*,#2014,.F.);
#2599=ORIENTED_EDGE('',*,*,#2015,.F.);
#2600=ORIENTED_EDGE('',*,*,#2016,.F.);
#2601=ORIENTED_EDGE('',*,*,#2017,.F.);
#2602=ORIENTED_EDGE('',*,*,#2018,.F.);
#2603=ORIENTED_EDGE('',*,*,#2019,.F.);
#2604=ORIENTED_EDGE('',*,*,#2005,.T.);
#2605=ORIENTED_EDGE('',*,*,#2020,.F.);
#2606=ORIENTED_EDGE('',*,*,#2021,.F.);
#2607=ORIENTED_EDGE('',*,*,#2022,.T.);
#2608=ORIENTED_EDGE('',*,*,#2023,.T.);
#2609=ORIENTED_EDGE('',*,*,#2024,.T.);
#2610=ORIENTED_EDGE('',*,*,#2025,.T.);
#2611=ORIENTED_EDGE('',*,*,#2026,.T.);
#2612=ORIENTED_EDGE('',*,*,#2027,.T.);
#2613=ORIENTED_EDGE('',*,*,#2022,.F.);
#2614=ORIENTED_EDGE('',*,*,#2028,.T.);
#2615=ORIENTED_EDGE('',*,*,#2026,.F.);
#2616=ORIENTED_EDGE('',*,*,#2029,.T.);
#2617=ORIENTED_EDGE('',*,*,#2030,.T.);
#2618=ORIENTED_EDGE('',*,*,#2031,.T.);
#2619=ORIENTED_EDGE('',*,*,#2032,.T.);
#2620=ORIENTED_EDGE('',*,*,#2033,.T.);
#2621=ORIENTED_EDGE('',*,*,#2030,.F.);
#2622=ORIENTED_EDGE('',*,*,#2034,.T.);
#2623=ORIENTED_EDGE('',*,*,#2035,.T.);
#2624=ORIENTED_EDGE('',*,*,#2036,.T.);
#2625=ORIENTED_EDGE('',*,*,#2037,.T.);
#2626=ORIENTED_EDGE('',*,*,#2038,.T.);
#2627=ORIENTED_EDGE('',*,*,#2010,.T.);
#2628=ORIENTED_EDGE('',*,*,#2036,.F.);
#2629=ORIENTED_EDGE('',*,*,#2039,.T.);
#2630=ORIENTED_EDGE('',*,*,#2038,.F.);
#2631=ORIENTED_EDGE('',*,*,#2040,.T.);
#2632=ORIENTED_EDGE('',*,*,#2024,.F.);
#2633=ORIENTED_EDGE('',*,*,#2011,.T.);
#2634=ORIENTED_EDGE('',*,*,#2033,.F.);
#2635=ORIENTED_EDGE('',*,*,#2041,.T.);
#2636=ORIENTED_EDGE('',*,*,#2042,.T.);
#2637=ORIENTED_EDGE('',*,*,#2043,.T.);
#2638=ORIENTED_EDGE('',*,*,#2028,.F.);
#2639=ORIENTED_EDGE('',*,*,#2044,.F.);
#2640=ORIENTED_EDGE('',*,*,#2045,.T.);
#2641=ORIENTED_EDGE('',*,*,#2032,.F.);
#2642=ORIENTED_EDGE('',*,*,#2029,.F.);
#2643=ORIENTED_EDGE('',*,*,#2044,.T.);
#2644=ORIENTED_EDGE('',*,*,#2025,.F.);
#2645=ORIENTED_EDGE('',*,*,#2040,.F.);
#2646=ORIENTED_EDGE('',*,*,#2046,.T.);
#2647=ORIENTED_EDGE('',*,*,#2039,.F.);
#2648=ORIENTED_EDGE('',*,*,#2035,.F.);
#2649=ORIENTED_EDGE('',*,*,#2047,.T.);
#2650=ORIENTED_EDGE('',*,*,#1997,.T.);
#2651=ORIENTED_EDGE('',*,*,#2004,.T.);
#2652=ORIENTED_EDGE('',*,*,#2048,.T.);
#2653=ORIENTED_EDGE('',*,*,#2049,.F.);
#2654=ORIENTED_EDGE('',*,*,#2050,.F.);
#2655=ORIENTED_EDGE('',*,*,#2051,.F.);
#2656=ORIENTED_EDGE('',*,*,#2052,.F.);
#2657=ORIENTED_EDGE('',*,*,#2053,.T.);
#2658=ORIENTED_EDGE('',*,*,#2041,.F.);
#2659=ORIENTED_EDGE('',*,*,#2046,.F.);
#2660=ORIENTED_EDGE('',*,*,#2054,.T.);
#2661=ORIENTED_EDGE('',*,*,#2055,.T.);
#2662=ORIENTED_EDGE('',*,*,#2056,.T.);
#2663=ORIENTED_EDGE('',*,*,#2057,.T.);
#2664=ORIENTED_EDGE('',*,*,#2058,.T.);
#2665=ORIENTED_EDGE('',*,*,#2059,.T.);
#2666=ORIENTED_EDGE('',*,*,#2056,.F.);
#2667=ORIENTED_EDGE('',*,*,#2008,.T.);
#2668=ORIENTED_EDGE('',*,*,#2060,.T.);
#2669=ORIENTED_EDGE('',*,*,#2061,.T.);
#2670=ORIENTED_EDGE('',*,*,#2062,.T.);
#2671=ORIENTED_EDGE('',*,*,#2063,.T.);
#2672=ORIENTED_EDGE('',*,*,#2064,.T.);
#2673=ORIENTED_EDGE('',*,*,#2065,.T.);
#2674=ORIENTED_EDGE('',*,*,#2060,.F.);
#2675=ORIENTED_EDGE('',*,*,#2066,.T.);
#2676=ORIENTED_EDGE('',*,*,#2067,.T.);
#2677=ORIENTED_EDGE('',*,*,#2068,.T.);
#2678=ORIENTED_EDGE('',*,*,#2064,.F.);
#2679=ORIENTED_EDGE('',*,*,#2069,.T.);
#2680=ORIENTED_EDGE('',*,*,#2067,.F.);
#2681=ORIENTED_EDGE('',*,*,#2070,.T.);
#2682=ORIENTED_EDGE('',*,*,#2071,.T.);
#2683=ORIENTED_EDGE('',*,*,#2062,.F.);
#2684=ORIENTED_EDGE('',*,*,#2072,.T.);
#2685=ORIENTED_EDGE('',*,*,#2058,.F.);
#2686=ORIENTED_EDGE('',*,*,#2007,.T.);
#2687=ORIENTED_EDGE('',*,*,#2065,.F.);
#2688=ORIENTED_EDGE('',*,*,#2073,.F.);
#2689=ORIENTED_EDGE('',*,*,#2074,.T.);
#2690=ORIENTED_EDGE('',*,*,#2070,.F.);
#2691=ORIENTED_EDGE('',*,*,#2075,.T.);
#2692=ORIENTED_EDGE('',*,*,#2018,.T.);
#2693=ORIENTED_EDGE('',*,*,#2076,.T.);
#2694=ORIENTED_EDGE('',*,*,#2069,.F.);
#2695=ORIENTED_EDGE('',*,*,#2066,.F.);
#2696=ORIENTED_EDGE('',*,*,#2063,.F.);
#2697=ORIENTED_EDGE('',*,*,#2006,.T.);
#2698=ORIENTED_EDGE('',*,*,#2019,.T.);
#2699=ORIENTED_EDGE('',*,*,#2075,.F.);
#2700=ORIENTED_EDGE('',*,*,#2077,.T.);
#2701=ORIENTED_EDGE('',*,*,#2078,.T.);
#2702=ORIENTED_EDGE('',*,*,#2079,.T.);
#2703=ORIENTED_EDGE('',*,*,#2077,.F.);
#2704=ORIENTED_EDGE('',*,*,#2080,.T.);
#2705=ORIENTED_EDGE('',*,*,#2081,.T.);
#2706=ORIENTED_EDGE('',*,*,#2082,.T.);
#2707=ORIENTED_EDGE('',*,*,#2083,.T.);
#2708=ORIENTED_EDGE('',*,*,#2084,.T.);
#2709=ORIENTED_EDGE('',*,*,#2081,.F.);
#2710=ORIENTED_EDGE('',*,*,#2085,.T.);
#2711=ORIENTED_EDGE('',*,*,#2086,.T.);
#2712=ORIENTED_EDGE('',*,*,#2087,.T.);
#2713=ORIENTED_EDGE('',*,*,#2083,.F.);
#2714=ORIENTED_EDGE('',*,*,#2088,.T.);
#2715=ORIENTED_EDGE('',*,*,#2089,.T.);
#2716=ORIENTED_EDGE('',*,*,#2090,.T.);
#2717=ORIENTED_EDGE('',*,*,#2082,.F.);
#2718=ORIENTED_EDGE('',*,*,#2084,.F.);
#2719=ORIENTED_EDGE('',*,*,#2087,.F.);
#2720=ORIENTED_EDGE('',*,*,#2091,.F.);
#2721=ORIENTED_EDGE('',*,*,#2092,.T.);
#2722=ORIENTED_EDGE('',*,*,#2093,.F.);
#2723=ORIENTED_EDGE('',*,*,#2086,.F.);
#2724=ORIENTED_EDGE('',*,*,#2094,.F.);
#2725=ORIENTED_EDGE('',*,*,#2095,.T.);
#2726=ORIENTED_EDGE('',*,*,#2096,.T.);
#2727=ORIENTED_EDGE('',*,*,#2091,.T.);
#2728=ORIENTED_EDGE('',*,*,#2090,.F.);
#2729=ORIENTED_EDGE('',*,*,#2097,.T.);
#2730=ORIENTED_EDGE('',*,*,#2094,.T.);
#2731=ORIENTED_EDGE('',*,*,#2089,.F.);
#2732=ORIENTED_EDGE('',*,*,#2098,.T.);
#2733=ORIENTED_EDGE('',*,*,#2099,.F.);
#2734=ORIENTED_EDGE('',*,*,#2100,.T.);
#2735=ORIENTED_EDGE('',*,*,#2095,.F.);
#2736=ORIENTED_EDGE('',*,*,#2097,.F.);
#2737=ORIENTED_EDGE('',*,*,#2101,.T.);
#2738=ORIENTED_EDGE('',*,*,#2102,.T.);
#2739=ORIENTED_EDGE('',*,*,#2103,.T.);
#2740=ORIENTED_EDGE('',*,*,#2104,.T.);
#2741=ORIENTED_EDGE('',*,*,#2101,.F.);
#2742=ORIENTED_EDGE('',*,*,#2105,.T.);
#2743=ORIENTED_EDGE('',*,*,#2106,.T.);
#2744=ORIENTED_EDGE('',*,*,#2107,.T.);
#2745=ORIENTED_EDGE('',*,*,#2108,.T.);
#2746=ORIENTED_EDGE('',*,*,#2109,.T.);
#2747=ORIENTED_EDGE('',*,*,#2106,.F.);
#2748=ORIENTED_EDGE('',*,*,#2110,.T.);
#2749=ORIENTED_EDGE('',*,*,#2111,.T.);
#2750=ORIENTED_EDGE('',*,*,#2103,.F.);
#2751=ORIENTED_EDGE('',*,*,#2112,.T.);
#2752=ORIENTED_EDGE('',*,*,#2113,.T.);
#2753=ORIENTED_EDGE('',*,*,#2114,.T.);
#2754=ORIENTED_EDGE('',*,*,#2109,.F.);
#2755=ORIENTED_EDGE('',*,*,#2115,.T.);
#2756=ORIENTED_EDGE('',*,*,#2016,.T.);
#2757=ORIENTED_EDGE('',*,*,#2116,.T.);
#2758=ORIENTED_EDGE('',*,*,#2108,.F.);
#2759=ORIENTED_EDGE('',*,*,#2105,.F.);
#2760=ORIENTED_EDGE('',*,*,#2117,.T.);
#2761=ORIENTED_EDGE('',*,*,#2111,.F.);
#2762=ORIENTED_EDGE('',*,*,#2118,.F.);
#2763=ORIENTED_EDGE('',*,*,#2119,.T.);
#2764=ORIENTED_EDGE('',*,*,#2114,.F.);
#2765=ORIENTED_EDGE('',*,*,#2120,.T.);
#2766=ORIENTED_EDGE('',*,*,#2121,.F.);
#2767=ORIENTED_EDGE('',*,*,#2104,.F.);
#2768=ORIENTED_EDGE('',*,*,#2117,.F.);
#2769=ORIENTED_EDGE('',*,*,#2122,.T.);
#2770=ORIENTED_EDGE('',*,*,#2110,.F.);
#2771=ORIENTED_EDGE('',*,*,#2121,.T.);
#2772=ORIENTED_EDGE('',*,*,#2123,.T.);
#2773=ORIENTED_EDGE('',*,*,#2124,.T.);
#2774=ORIENTED_EDGE('',*,*,#2125,.F.);
#2775=ORIENTED_EDGE('',*,*,#2118,.T.);
#2776=ORIENTED_EDGE('',*,*,#2125,.T.);
#2777=ORIENTED_EDGE('',*,*,#2126,.T.);
#2778=ORIENTED_EDGE('',*,*,#2127,.T.);
#2779=ORIENTED_EDGE('',*,*,#2128,.T.);
#2780=ORIENTED_EDGE('',*,*,#2129,.T.);
#2781=ORIENTED_EDGE('',*,*,#2130,.T.);
#2782=ORIENTED_EDGE('',*,*,#2131,.T.);
#2783=ORIENTED_EDGE('',*,*,#2132,.T.);
#2784=ORIENTED_EDGE('',*,*,#2133,.T.);
#2785=ORIENTED_EDGE('',*,*,#2134,.T.);
#2786=ORIENTED_EDGE('',*,*,#2130,.F.);
#2787=ORIENTED_EDGE('',*,*,#2135,.T.);
#2788=ORIENTED_EDGE('',*,*,#2136,.T.);
#2789=ORIENTED_EDGE('',*,*,#2137,.T.);
#2790=ORIENTED_EDGE('',*,*,#2138,.T.);
#2791=ORIENTED_EDGE('',*,*,#2139,.T.);
#2792=ORIENTED_EDGE('',*,*,#2132,.F.);
#2793=ORIENTED_EDGE('',*,*,#2140,.T.);
#2794=ORIENTED_EDGE('',*,*,#2141,.T.);
#2795=ORIENTED_EDGE('',*,*,#2137,.F.);
#2796=ORIENTED_EDGE('',*,*,#2142,.T.);
#2797=ORIENTED_EDGE('',*,*,#2143,.T.);
#2798=ORIENTED_EDGE('',*,*,#2140,.F.);
#2799=ORIENTED_EDGE('',*,*,#2144,.T.);
#2800=ORIENTED_EDGE('',*,*,#2145,.T.);
#2801=ORIENTED_EDGE('',*,*,#2146,.T.);
#2802=ORIENTED_EDGE('',*,*,#2147,.T.);
#2803=ORIENTED_EDGE('',*,*,#2148,.T.);
#2804=ORIENTED_EDGE('',*,*,#2149,.T.);
#2805=ORIENTED_EDGE('',*,*,#2145,.F.);
#2806=ORIENTED_EDGE('',*,*,#2150,.T.);
#2807=ORIENTED_EDGE('',*,*,#2151,.T.);
#2808=ORIENTED_EDGE('',*,*,#2148,.F.);
#2809=ORIENTED_EDGE('',*,*,#2152,.T.);
#2810=ORIENTED_EDGE('',*,*,#2153,.T.);
#2811=ORIENTED_EDGE('',*,*,#2154,.T.);
#2812=ORIENTED_EDGE('',*,*,#2099,.T.);
#2813=ORIENTED_EDGE('',*,*,#2050,.T.);
#2814=ORIENTED_EDGE('',*,*,#2153,.F.);
#2815=ORIENTED_EDGE('',*,*,#2155,.T.);
#2816=ORIENTED_EDGE('',*,*,#2133,.F.);
#2817=ORIENTED_EDGE('',*,*,#2150,.F.);
#2818=ORIENTED_EDGE('',*,*,#2156,.T.);
#2819=ORIENTED_EDGE('',*,*,#2127,.F.);
#2820=ORIENTED_EDGE('',*,*,#2107,.F.);
#2821=ORIENTED_EDGE('',*,*,#2116,.F.);
#2822=ORIENTED_EDGE('',*,*,#2015,.T.);
#2823=ORIENTED_EDGE('',*,*,#2157,.T.);
#2824=ORIENTED_EDGE('',*,*,#2112,.F.);
#2825=ORIENTED_EDGE('',*,*,#2102,.F.);
#2826=ORIENTED_EDGE('',*,*,#2059,.F.);
#2827=ORIENTED_EDGE('',*,*,#2158,.F.);
#2828=ORIENTED_EDGE('',*,*,#2076,.F.);
#2829=ORIENTED_EDGE('',*,*,#2017,.T.);
#2830=ORIENTED_EDGE('',*,*,#2115,.F.);
#2831=ORIENTED_EDGE('',*,*,#2119,.F.);
#2832=ORIENTED_EDGE('',*,*,#2128,.F.);
#2833=ORIENTED_EDGE('',*,*,#2159,.F.);
#2834=ORIENTED_EDGE('',*,*,#2160,.T.);
#2835=ORIENTED_EDGE('',*,*,#2161,.T.);
#2836=ORIENTED_EDGE('',*,*,#1999,.T.);
#2837=ORIENTED_EDGE('',*,*,#2162,.T.);
#2838=ORIENTED_EDGE('',*,*,#2057,.F.);
#2839=ORIENTED_EDGE('',*,*,#2156,.F.);
#2840=ORIENTED_EDGE('',*,*,#2163,.T.);
#2841=ORIENTED_EDGE('',*,*,#2164,.T.);
#2842=ORIENTED_EDGE('',*,*,#2159,.T.);
#2843=ORIENTED_EDGE('',*,*,#2152,.F.);
#2844=ORIENTED_EDGE('',*,*,#2165,.F.);
#2845=ORIENTED_EDGE('',*,*,#2166,.F.);
#2846=ORIENTED_EDGE('',*,*,#2163,.F.);
#2847=ORIENTED_EDGE('',*,*,#2147,.F.);
#2848=ORIENTED_EDGE('',*,*,#2144,.F.);
#2849=ORIENTED_EDGE('',*,*,#2167,.F.);
#2850=ORIENTED_EDGE('',*,*,#2168,.F.);
#2851=ORIENTED_EDGE('',*,*,#2165,.T.);
#2852=ORIENTED_EDGE('',*,*,#2142,.F.);
#2853=ORIENTED_EDGE('',*,*,#2169,.F.);
#2854=ORIENTED_EDGE('',*,*,#2170,.F.);
#2855=ORIENTED_EDGE('',*,*,#2167,.T.);
#2856=ORIENTED_EDGE('',*,*,#2136,.F.);
#2857=ORIENTED_EDGE('',*,*,#2131,.F.);
#2858=ORIENTED_EDGE('',*,*,#2171,.F.);
#2859=ORIENTED_EDGE('',*,*,#2172,.F.);
#2860=ORIENTED_EDGE('',*,*,#2169,.T.);
#2861=ORIENTED_EDGE('',*,*,#2134,.F.);
#2862=ORIENTED_EDGE('',*,*,#2173,.F.);
#2863=ORIENTED_EDGE('',*,*,#2174,.F.);
#2864=ORIENTED_EDGE('',*,*,#2171,.T.);
#2865=ORIENTED_EDGE('',*,*,#2155,.F.);
#2866=ORIENTED_EDGE('',*,*,#2049,.T.);
#2867=ORIENTED_EDGE('',*,*,#2175,.T.);
#2868=ORIENTED_EDGE('',*,*,#2173,.T.);
#2869=ORIENTED_EDGE('',*,*,#1983,.T.);
#2870=ORIENTED_EDGE('',*,*,#2176,.F.);
#2871=ORIENTED_EDGE('',*,*,#2160,.F.);
#2872=ORIENTED_EDGE('',*,*,#2164,.F.);
#2873=ORIENTED_EDGE('',*,*,#2166,.T.);
#2874=ORIENTED_EDGE('',*,*,#2168,.T.);
#2875=ORIENTED_EDGE('',*,*,#2170,.T.);
#2876=ORIENTED_EDGE('',*,*,#2172,.T.);
#2877=ORIENTED_EDGE('',*,*,#2174,.T.);
#2878=ORIENTED_EDGE('',*,*,#2175,.F.);
#2879=ORIENTED_EDGE('',*,*,#2048,.F.);
#2880=ORIENTED_EDGE('',*,*,#2003,.F.);
#2881=ORIENTED_EDGE('',*,*,#1990,.T.);
#2882=ORIENTED_EDGE('',*,*,#1975,.T.);
#2883=ORIENTED_EDGE('',*,*,#2177,.T.);
#2884=ORIENTED_EDGE('',*,*,#2178,.F.);
#2885=ORIENTED_EDGE('',*,*,#2179,.F.);
#2886=ORIENTED_EDGE('',*,*,#2180,.T.);
#2887=ORIENTED_EDGE('',*,*,#2177,.F.);
#2888=ORIENTED_EDGE('',*,*,#2180,.F.);
#2889=ORIENTED_EDGE('',*,*,#2143,.F.);
#2890=ORIENTED_EDGE('',*,*,#2181,.T.);
#2891=ORIENTED_EDGE('',*,*,#2179,.T.);
#2892=ORIENTED_EDGE('',*,*,#2182,.T.);
#2893=ORIENTED_EDGE('',*,*,#2138,.F.);
#2894=ORIENTED_EDGE('',*,*,#2141,.F.);
#2895=ORIENTED_EDGE('',*,*,#2078,.F.);
#2896=ORIENTED_EDGE('',*,*,#2093,.T.);
#2897=ORIENTED_EDGE('',*,*,#2183,.T.);
#2898=ORIENTED_EDGE('',*,*,#2052,.T.);
#2899=ORIENTED_EDGE('',*,*,#2079,.F.);
#2900=ORIENTED_EDGE('',*,*,#2051,.T.);
#2901=ORIENTED_EDGE('',*,*,#2098,.F.);
#2902=ORIENTED_EDGE('',*,*,#2088,.F.);
#2903=ORIENTED_EDGE('',*,*,#2184,.T.);
#2904=ORIENTED_EDGE('',*,*,#2080,.F.);
#2905=ORIENTED_EDGE('',*,*,#2085,.F.);
#2906=ORIENTED_EDGE('',*,*,#2184,.F.);
#2907=ORIENTED_EDGE('',*,*,#2185,.T.);
#2908=ORIENTED_EDGE('',*,*,#2061,.F.);
#2909=ORIENTED_EDGE('',*,*,#2073,.T.);
#2910=ORIENTED_EDGE('',*,*,#2068,.F.);
#2911=ORIENTED_EDGE('',*,*,#2071,.F.);
#2912=ORIENTED_EDGE('',*,*,#2158,.T.);
#2913=ORIENTED_EDGE('',*,*,#2072,.F.);
#2914=ORIENTED_EDGE('',*,*,#2045,.F.);
#2915=ORIENTED_EDGE('',*,*,#2186,.T.);
#2916=ORIENTED_EDGE('',*,*,#2187,.T.);
#2917=ORIENTED_EDGE('',*,*,#2186,.F.);
#2918=ORIENTED_EDGE('',*,*,#2031,.F.);
#2919=ORIENTED_EDGE('',*,*,#2043,.F.);
#2920=ORIENTED_EDGE('',*,*,#2188,.T.);
#2921=ORIENTED_EDGE('',*,*,#2012,.T.);
#2922=ORIENTED_EDGE('',*,*,#2023,.F.);
#2923=ORIENTED_EDGE('',*,*,#2027,.F.);
#2924=ORIENTED_EDGE('',*,*,#2074,.F.);
#2925=ORIENTED_EDGE('',*,*,#2189,.T.);
#2926=ORIENTED_EDGE('',*,*,#2020,.T.);
#2927=ORIENTED_EDGE('',*,*,#2189,.F.);
#2928=ORIENTED_EDGE('',*,*,#2185,.F.);
#2929=ORIENTED_EDGE('',*,*,#2190,.T.);
#2930=ORIENTED_EDGE('',*,*,#2191,.T.);
#2931=ORIENTED_EDGE('',*,*,#2190,.F.);
#2932=ORIENTED_EDGE('',*,*,#2122,.F.);
#2933=ORIENTED_EDGE('',*,*,#2192,.T.);
#2934=ORIENTED_EDGE('',*,*,#2021,.T.);
#2935=ORIENTED_EDGE('',*,*,#2192,.F.);
#2936=ORIENTED_EDGE('',*,*,#2113,.F.);
#2937=ORIENTED_EDGE('',*,*,#2157,.F.);
#2938=ORIENTED_EDGE('',*,*,#2193,.T.);
#2939=ORIENTED_EDGE('',*,*,#2123,.F.);
#2940=ORIENTED_EDGE('',*,*,#2120,.F.);
#2941=ORIENTED_EDGE('',*,*,#2194,.F.);
#2942=ORIENTED_EDGE('',*,*,#2195,.T.);
#2943=ORIENTED_EDGE('',*,*,#2195,.F.);
#2944=ORIENTED_EDGE('',*,*,#2002,.F.);
#2945=ORIENTED_EDGE('',*,*,#2196,.T.);
#2946=ORIENTED_EDGE('',*,*,#2194,.T.);
#2947=ORIENTED_EDGE('',*,*,#2196,.F.);
#2948=ORIENTED_EDGE('',*,*,#2197,.F.);
#2949=ORIENTED_EDGE('',*,*,#2198,.T.);
#2950=ORIENTED_EDGE('',*,*,#2198,.F.);
#2951=ORIENTED_EDGE('',*,*,#2001,.F.);
#2952=ORIENTED_EDGE('',*,*,#2199,.T.);
#2953=ORIENTED_EDGE('',*,*,#2197,.T.);
#2954=ORIENTED_EDGE('',*,*,#2199,.F.);
#2955=ORIENTED_EDGE('',*,*,#1982,.T.);
#2956=ORIENTED_EDGE('',*,*,#2000,.F.);
#2957=ORIENTED_EDGE('',*,*,#2161,.F.);
#2958=ORIENTED_EDGE('',*,*,#2176,.T.);
#2959=ORIENTED_EDGE('',*,*,#2034,.F.);
#2960=ORIENTED_EDGE('',*,*,#2200,.F.);
#2961=ORIENTED_EDGE('',*,*,#2054,.F.);
#2962=ORIENTED_EDGE('',*,*,#2162,.F.);
#2963=ORIENTED_EDGE('',*,*,#1998,.T.);
#2964=ORIENTED_EDGE('',*,*,#2047,.F.);
#2965=ORIENTED_EDGE('',*,*,#2037,.F.);
#2966=ORIENTED_EDGE('',*,*,#2009,.F.);
#2967=ORIENTED_EDGE('',*,*,#2055,.F.);
#2968=ORIENTED_EDGE('',*,*,#2200,.T.);
#2969=ORIENTED_EDGE('',*,*,#1971,.T.);
#2970=ORIENTED_EDGE('',*,*,#2013,.T.);
#2971=ORIENTED_EDGE('',*,*,#2188,.F.);
#2972=ORIENTED_EDGE('',*,*,#2042,.F.);
#2973=ORIENTED_EDGE('',*,*,#2053,.F.);
#2974=ORIENTED_EDGE('',*,*,#2183,.F.);
#2975=ORIENTED_EDGE('',*,*,#2092,.F.);
#2976=ORIENTED_EDGE('',*,*,#2201,.F.);
#2977=ORIENTED_EDGE('',*,*,#2187,.F.);
#2978=ORIENTED_EDGE('',*,*,#2191,.F.);
#2979=ORIENTED_EDGE('',*,*,#1972,.T.);
#2980=ORIENTED_EDGE('',*,*,#2201,.T.);
#2981=ORIENTED_EDGE('',*,*,#2096,.F.);
#2982=ORIENTED_EDGE('',*,*,#2100,.F.);
#2983=ORIENTED_EDGE('',*,*,#2154,.F.);
#2984=ORIENTED_EDGE('',*,*,#2135,.F.);
#2985=ORIENTED_EDGE('',*,*,#2129,.F.);
#2986=ORIENTED_EDGE('',*,*,#2139,.F.);
#2987=ORIENTED_EDGE('',*,*,#2182,.F.);
#2988=ORIENTED_EDGE('',*,*,#2178,.T.);
#2989=ORIENTED_EDGE('',*,*,#2181,.F.);
#2990=ORIENTED_EDGE('',*,*,#2146,.F.);
#2991=ORIENTED_EDGE('',*,*,#2149,.F.);
#2992=ORIENTED_EDGE('',*,*,#2151,.F.);
#2993=ORIENTED_EDGE('',*,*,#2126,.F.);
#2994=ORIENTED_EDGE('',*,*,#2124,.F.);
#2995=ORIENTED_EDGE('',*,*,#2193,.F.);
#2996=ORIENTED_EDGE('',*,*,#2014,.T.);
#2997=ORIENTED_EDGE('',*,*,#1969,.T.);
#2998=ORIENTED_EDGE('',*,*,#1966,.T.);
#2999=ORIENTED_EDGE('',*,*,#1984,.T.);
#3000=ORIENTED_EDGE('',*,*,#1977,.T.);
#3001=ORIENTED_EDGE('',*,*,#1989,.T.);
#3002=ORIENTED_EDGE('',*,*,#1986,.T.);
#3003=ORIENTED_EDGE('',*,*,#2202,.F.);
#3004=ORIENTED_EDGE('',*,*,#2203,.T.);
#3005=ORIENTED_EDGE('',*,*,#2204,.T.);
#3006=ORIENTED_EDGE('',*,*,#2203,.F.);
#3007=ORIENTED_EDGE('',*,*,#2204,.F.);
#3008=ORIENTED_EDGE('',*,*,#2205,.F.);
#3009=ORIENTED_EDGE('',*,*,#2206,.T.);
#3010=ORIENTED_EDGE('',*,*,#2207,.T.);
#3011=ORIENTED_EDGE('',*,*,#2206,.F.);
#3012=ORIENTED_EDGE('',*,*,#2207,.F.);
#3013=ORIENTED_EDGE('',*,*,#2208,.T.);
#3014=ORIENTED_EDGE('',*,*,#2209,.T.);
#3015=ORIENTED_EDGE('',*,*,#2210,.T.);
#3016=ORIENTED_EDGE('',*,*,#2211,.T.);
#3017=ORIENTED_EDGE('',*,*,#2212,.T.);
#3018=ORIENTED_EDGE('',*,*,#2213,.T.);
#3019=ORIENTED_EDGE('',*,*,#2208,.F.);
#3020=ORIENTED_EDGE('',*,*,#2214,.T.);
#3021=ORIENTED_EDGE('',*,*,#2215,.T.);
#3022=ORIENTED_EDGE('',*,*,#2216,.T.);
#3023=ORIENTED_EDGE('',*,*,#2212,.F.);
#3024=ORIENTED_EDGE('',*,*,#2217,.T.);
#3025=ORIENTED_EDGE('',*,*,#2218,.T.);
#3026=ORIENTED_EDGE('',*,*,#2219,.T.);
#3027=ORIENTED_EDGE('',*,*,#2215,.F.);
#3028=ORIENTED_EDGE('',*,*,#2220,.T.);
#3029=ORIENTED_EDGE('',*,*,#2221,.T.);
#3030=ORIENTED_EDGE('',*,*,#2222,.T.);
#3031=ORIENTED_EDGE('',*,*,#2218,.F.);
#3032=ORIENTED_EDGE('',*,*,#2223,.T.);
#3033=ORIENTED_EDGE('',*,*,#2224,.T.);
#3034=ORIENTED_EDGE('',*,*,#2225,.T.);
#3035=ORIENTED_EDGE('',*,*,#2221,.F.);
#3036=ORIENTED_EDGE('',*,*,#2226,.T.);
#3037=ORIENTED_EDGE('',*,*,#2227,.T.);
#3038=ORIENTED_EDGE('',*,*,#2228,.T.);
#3039=ORIENTED_EDGE('',*,*,#2224,.F.);
#3040=ORIENTED_EDGE('',*,*,#2229,.T.);
#3041=ORIENTED_EDGE('',*,*,#2230,.T.);
#3042=ORIENTED_EDGE('',*,*,#2231,.T.);
#3043=ORIENTED_EDGE('',*,*,#2227,.F.);
#3044=ORIENTED_EDGE('',*,*,#2232,.T.);
#3045=ORIENTED_EDGE('',*,*,#2233,.T.);
#3046=ORIENTED_EDGE('',*,*,#2234,.T.);
#3047=ORIENTED_EDGE('',*,*,#2230,.F.);
#3048=ORIENTED_EDGE('',*,*,#2235,.T.);
#3049=ORIENTED_EDGE('',*,*,#2236,.T.);
#3050=ORIENTED_EDGE('',*,*,#2237,.T.);
#3051=ORIENTED_EDGE('',*,*,#2238,.T.);
#3052=ORIENTED_EDGE('',*,*,#2233,.F.);
#3053=ORIENTED_EDGE('',*,*,#2239,.F.);
#3054=ORIENTED_EDGE('',*,*,#2240,.T.);
#3055=ORIENTED_EDGE('',*,*,#2237,.F.);
#3056=ORIENTED_EDGE('',*,*,#2241,.T.);
#3057=ORIENTED_EDGE('',*,*,#2235,.F.);
#3058=ORIENTED_EDGE('',*,*,#2232,.F.);
#3059=ORIENTED_EDGE('',*,*,#2229,.F.);
#3060=ORIENTED_EDGE('',*,*,#2226,.F.);
#3061=ORIENTED_EDGE('',*,*,#2242,.F.);
#3062=ORIENTED_EDGE('',*,*,#2243,.T.);
#3063=ORIENTED_EDGE('',*,*,#2223,.F.);
#3064=ORIENTED_EDGE('',*,*,#2244,.T.);
#3065=ORIENTED_EDGE('',*,*,#2245,.T.);
#3066=ORIENTED_EDGE('',*,*,#2246,.T.);
#3067=ORIENTED_EDGE('',*,*,#2247,.T.);
#3068=ORIENTED_EDGE('',*,*,#2242,.T.);
#3069=ORIENTED_EDGE('',*,*,#2220,.F.);
#3070=ORIENTED_EDGE('',*,*,#2217,.F.);
#3071=ORIENTED_EDGE('',*,*,#2214,.F.);
#3072=ORIENTED_EDGE('',*,*,#2211,.F.);
#3073=ORIENTED_EDGE('',*,*,#2248,.T.);
#3074=ORIENTED_EDGE('',*,*,#2244,.F.);
#3075=ORIENTED_EDGE('',*,*,#2249,.T.);
#3076=ORIENTED_EDGE('',*,*,#2250,.T.);
#3077=ORIENTED_EDGE('',*,*,#2251,.T.);
#3078=ORIENTED_EDGE('',*,*,#2252,.T.);
#3079=ORIENTED_EDGE('',*,*,#2253,.T.);
#3080=ORIENTED_EDGE('',*,*,#2254,.T.);
#3081=ORIENTED_EDGE('',*,*,#2251,.F.);
#3082=ORIENTED_EDGE('',*,*,#2255,.T.);
#3083=ORIENTED_EDGE('',*,*,#2256,.T.);
#3084=ORIENTED_EDGE('',*,*,#2257,.T.);
#3085=ORIENTED_EDGE('',*,*,#2253,.F.);
#3086=ORIENTED_EDGE('',*,*,#2258,.T.);
#3087=ORIENTED_EDGE('',*,*,#2259,.T.);
#3088=ORIENTED_EDGE('',*,*,#2260,.T.);
#3089=ORIENTED_EDGE('',*,*,#2256,.F.);
#3090=ORIENTED_EDGE('',*,*,#2261,.T.);
#3091=ORIENTED_EDGE('',*,*,#2262,.T.);
#3092=ORIENTED_EDGE('',*,*,#2263,.T.);
#3093=ORIENTED_EDGE('',*,*,#2259,.F.);
#3094=ORIENTED_EDGE('',*,*,#2264,.T.);
#3095=ORIENTED_EDGE('',*,*,#2265,.T.);
#3096=ORIENTED_EDGE('',*,*,#2266,.T.);
#3097=ORIENTED_EDGE('',*,*,#2262,.F.);
#3098=ORIENTED_EDGE('',*,*,#2267,.T.);
#3099=ORIENTED_EDGE('',*,*,#2268,.T.);
#3100=ORIENTED_EDGE('',*,*,#2269,.T.);
#3101=ORIENTED_EDGE('',*,*,#2265,.F.);
#3102=ORIENTED_EDGE('',*,*,#2270,.T.);
#3103=ORIENTED_EDGE('',*,*,#2271,.T.);
#3104=ORIENTED_EDGE('',*,*,#2272,.T.);
#3105=ORIENTED_EDGE('',*,*,#2268,.F.);
#3106=ORIENTED_EDGE('',*,*,#2273,.T.);
#3107=ORIENTED_EDGE('',*,*,#2274,.T.);
#3108=ORIENTED_EDGE('',*,*,#2275,.T.);
#3109=ORIENTED_EDGE('',*,*,#2271,.F.);
#3110=ORIENTED_EDGE('',*,*,#2276,.T.);
#3111=ORIENTED_EDGE('',*,*,#2239,.T.);
#3112=ORIENTED_EDGE('',*,*,#2277,.T.);
#3113=ORIENTED_EDGE('',*,*,#2278,.T.);
#3114=ORIENTED_EDGE('',*,*,#2279,.F.);
#3115=ORIENTED_EDGE('',*,*,#2276,.F.);
#3116=ORIENTED_EDGE('',*,*,#2280,.T.);
#3117=ORIENTED_EDGE('',*,*,#2240,.F.);
#3118=ORIENTED_EDGE('',*,*,#2238,.F.);
#3119=ORIENTED_EDGE('',*,*,#2280,.F.);
#3120=ORIENTED_EDGE('',*,*,#2273,.F.);
#3121=ORIENTED_EDGE('',*,*,#2281,.T.);
#3122=ORIENTED_EDGE('',*,*,#2234,.F.);
#3123=ORIENTED_EDGE('',*,*,#2231,.F.);
#3124=ORIENTED_EDGE('',*,*,#2281,.F.);
#3125=ORIENTED_EDGE('',*,*,#2270,.F.);
#3126=ORIENTED_EDGE('',*,*,#2282,.T.);
#3127=ORIENTED_EDGE('',*,*,#2228,.F.);
#3128=ORIENTED_EDGE('',*,*,#2282,.F.);
#3129=ORIENTED_EDGE('',*,*,#2267,.F.);
#3130=ORIENTED_EDGE('',*,*,#2283,.T.);
#3131=ORIENTED_EDGE('',*,*,#2225,.F.);
#3132=ORIENTED_EDGE('',*,*,#2283,.F.);
#3133=ORIENTED_EDGE('',*,*,#2264,.F.);
#3134=ORIENTED_EDGE('',*,*,#2284,.T.);
#3135=ORIENTED_EDGE('',*,*,#2219,.F.);
#3136=ORIENTED_EDGE('',*,*,#2222,.F.);
#3137=ORIENTED_EDGE('',*,*,#2216,.F.);
#3138=ORIENTED_EDGE('',*,*,#2284,.F.);
#3139=ORIENTED_EDGE('',*,*,#2261,.F.);
#3140=ORIENTED_EDGE('',*,*,#2285,.T.);
#3141=ORIENTED_EDGE('',*,*,#2213,.F.);
#3142=ORIENTED_EDGE('',*,*,#2285,.F.);
#3143=ORIENTED_EDGE('',*,*,#2258,.F.);
#3144=ORIENTED_EDGE('',*,*,#2286,.T.);
#3145=ORIENTED_EDGE('',*,*,#2209,.F.);
#3146=ORIENTED_EDGE('',*,*,#2286,.F.);
#3147=ORIENTED_EDGE('',*,*,#2255,.F.);
#3148=ORIENTED_EDGE('',*,*,#2287,.T.);
#3149=ORIENTED_EDGE('',*,*,#2288,.T.);
#3150=ORIENTED_EDGE('',*,*,#2289,.T.);
#3151=ORIENTED_EDGE('',*,*,#2250,.F.);
#3152=ORIENTED_EDGE('',*,*,#2290,.T.);
#3153=ORIENTED_EDGE('',*,*,#2291,.T.);
#3154=ORIENTED_EDGE('',*,*,#2292,.T.);
#3155=ORIENTED_EDGE('',*,*,#2287,.F.);
#3156=ORIENTED_EDGE('',*,*,#2249,.F.);
#3157=ORIENTED_EDGE('',*,*,#2293,.F.);
#3158=ORIENTED_EDGE('',*,*,#2294,.T.);
#3159=ORIENTED_EDGE('',*,*,#2295,.T.);
#3160=ORIENTED_EDGE('',*,*,#2290,.F.);
#3161=ORIENTED_EDGE('',*,*,#2247,.F.);
#3162=ORIENTED_EDGE('',*,*,#2296,.F.);
#3163=ORIENTED_EDGE('',*,*,#2297,.T.);
#3164=ORIENTED_EDGE('',*,*,#2277,.F.);
#3165=ORIENTED_EDGE('',*,*,#2241,.F.);
#3166=ORIENTED_EDGE('',*,*,#2236,.F.);
#3167=ORIENTED_EDGE('',*,*,#2243,.F.);
#3168=ORIENTED_EDGE('',*,*,#2246,.F.);
#3169=ORIENTED_EDGE('',*,*,#2298,.F.);
#3170=ORIENTED_EDGE('',*,*,#2299,.F.);
#3171=ORIENTED_EDGE('',*,*,#2296,.T.);
#3172=ORIENTED_EDGE('',*,*,#2245,.F.);
#3173=ORIENTED_EDGE('',*,*,#2248,.F.);
#3174=ORIENTED_EDGE('',*,*,#2210,.F.);
#3175=ORIENTED_EDGE('',*,*,#2289,.F.);
#3176=ORIENTED_EDGE('',*,*,#2300,.F.);
#3177=ORIENTED_EDGE('',*,*,#2298,.T.);
#3178=ORIENTED_EDGE('',*,*,#2297,.F.);
#3179=ORIENTED_EDGE('',*,*,#2299,.T.);
#3180=ORIENTED_EDGE('',*,*,#2300,.T.);
#3181=ORIENTED_EDGE('',*,*,#2288,.F.);
#3182=ORIENTED_EDGE('',*,*,#2292,.F.);
#3183=ORIENTED_EDGE('',*,*,#2301,.T.);
#3184=ORIENTED_EDGE('',*,*,#2202,.T.);
#3185=ORIENTED_EDGE('',*,*,#2205,.T.);
#3186=ORIENTED_EDGE('',*,*,#2291,.F.);
#3187=ORIENTED_EDGE('',*,*,#2295,.F.);
#3188=ORIENTED_EDGE('',*,*,#2302,.F.);
#3189=ORIENTED_EDGE('',*,*,#2303,.T.);
#3190=ORIENTED_EDGE('',*,*,#2304,.F.);
#3191=ORIENTED_EDGE('',*,*,#2305,.F.);
#3192=ORIENTED_EDGE('',*,*,#2278,.F.);
#3193=ORIENTED_EDGE('',*,*,#2301,.F.);
#3194=ORIENTED_EDGE('',*,*,#2306,.F.);
#3195=ORIENTED_EDGE('',*,*,#2307,.T.);
#3196=ORIENTED_EDGE('',*,*,#2308,.F.);
#3197=ORIENTED_EDGE('',*,*,#2303,.F.);
#3198=ORIENTED_EDGE('',*,*,#2309,.F.);
#3199=ORIENTED_EDGE('',*,*,#2310,.T.);
#3200=ORIENTED_EDGE('',*,*,#2311,.F.);
#3201=ORIENTED_EDGE('',*,*,#2307,.F.);
#3202=ORIENTED_EDGE('',*,*,#2312,.F.);
#3203=ORIENTED_EDGE('',*,*,#2313,.F.);
#3204=ORIENTED_EDGE('',*,*,#2314,.F.);
#3205=ORIENTED_EDGE('',*,*,#2315,.T.);
#3206=ORIENTED_EDGE('',*,*,#2316,.F.);
#3207=ORIENTED_EDGE('',*,*,#2317,.F.);
#3208=ORIENTED_EDGE('',*,*,#2318,.F.);
#3209=ORIENTED_EDGE('',*,*,#2310,.F.);
#3210=ORIENTED_EDGE('',*,*,#2274,.F.);
#3211=ORIENTED_EDGE('',*,*,#2279,.T.);
#3212=ORIENTED_EDGE('',*,*,#2305,.T.);
#3213=ORIENTED_EDGE('',*,*,#2319,.F.);
#3214=ORIENTED_EDGE('',*,*,#2320,.T.);
#3215=ORIENTED_EDGE('',*,*,#2304,.T.);
#3216=ORIENTED_EDGE('',*,*,#2308,.T.);
#3217=ORIENTED_EDGE('',*,*,#2311,.T.);
#3218=ORIENTED_EDGE('',*,*,#2318,.T.);
#3219=ORIENTED_EDGE('',*,*,#2321,.F.);
#3220=ORIENTED_EDGE('',*,*,#2322,.T.);
#3221=ORIENTED_EDGE('',*,*,#2319,.T.);
#3222=ORIENTED_EDGE('',*,*,#2317,.T.);
#3223=ORIENTED_EDGE('',*,*,#2323,.F.);
#3224=ORIENTED_EDGE('',*,*,#2324,.T.);
#3225=ORIENTED_EDGE('',*,*,#2321,.T.);
#3226=ORIENTED_EDGE('',*,*,#2316,.T.);
#3227=ORIENTED_EDGE('',*,*,#2325,.F.);
#3228=ORIENTED_EDGE('',*,*,#2326,.T.);
#3229=ORIENTED_EDGE('',*,*,#2323,.T.);
#3230=ORIENTED_EDGE('',*,*,#2327,.F.);
#3231=ORIENTED_EDGE('',*,*,#2328,.T.);
#3232=ORIENTED_EDGE('',*,*,#2328,.F.);
#3233=ORIENTED_EDGE('',*,*,#2329,.F.);
#3234=ORIENTED_EDGE('',*,*,#2330,.T.);
#3235=ORIENTED_EDGE('',*,*,#2327,.T.);
#3236=ORIENTED_EDGE('',*,*,#2330,.F.);
#3237=ORIENTED_EDGE('',*,*,#2331,.F.);
#3238=ORIENTED_EDGE('',*,*,#2332,.T.);
#3239=ORIENTED_EDGE('',*,*,#2333,.T.);
#3240=ORIENTED_EDGE('',*,*,#2332,.F.);
#3241=ORIENTED_EDGE('',*,*,#2333,.F.);
#3242=ORIENTED_EDGE('',*,*,#2334,.F.);
#3243=ORIENTED_EDGE('',*,*,#2335,.T.);
#3244=ORIENTED_EDGE('',*,*,#2336,.F.);
#3245=ORIENTED_EDGE('',*,*,#2337,.F.);
#3246=ORIENTED_EDGE('',*,*,#2338,.F.);
#3247=ORIENTED_EDGE('',*,*,#2337,.T.);
#3248=ORIENTED_EDGE('',*,*,#2339,.F.);
#3249=ORIENTED_EDGE('',*,*,#2340,.F.);
#3250=ORIENTED_EDGE('',*,*,#2341,.F.);
#3251=ORIENTED_EDGE('',*,*,#2342,.F.);
#3252=ORIENTED_EDGE('',*,*,#2340,.T.);
#3253=ORIENTED_EDGE('',*,*,#2343,.F.);
#3254=ORIENTED_EDGE('',*,*,#2344,.F.);
#3255=ORIENTED_EDGE('',*,*,#2345,.T.);
#3256=ORIENTED_EDGE('',*,*,#2325,.T.);
#3257=ORIENTED_EDGE('',*,*,#2315,.F.);
#3258=ORIENTED_EDGE('',*,*,#2314,.T.);
#3259=ORIENTED_EDGE('',*,*,#2346,.F.);
#3260=ORIENTED_EDGE('',*,*,#2347,.F.);
#3261=ORIENTED_EDGE('',*,*,#2341,.T.);
#3262=ORIENTED_EDGE('',*,*,#2313,.T.);
#3263=ORIENTED_EDGE('',*,*,#2348,.F.);
#3264=ORIENTED_EDGE('',*,*,#2349,.F.);
#3265=ORIENTED_EDGE('',*,*,#2346,.T.);
#3266=ORIENTED_EDGE('',*,*,#2302,.T.);
#3267=ORIENTED_EDGE('',*,*,#2294,.F.);
#3268=ORIENTED_EDGE('',*,*,#2350,.F.);
#3269=ORIENTED_EDGE('',*,*,#2348,.T.);
#3270=ORIENTED_EDGE('',*,*,#2312,.T.);
#3271=ORIENTED_EDGE('',*,*,#2309,.T.);
#3272=ORIENTED_EDGE('',*,*,#2306,.T.);
#3273=ORIENTED_EDGE('',*,*,#2351,.T.);
#3274=ORIENTED_EDGE('',*,*,#2344,.T.);
#3275=ORIENTED_EDGE('',*,*,#2352,.F.);
#3276=ORIENTED_EDGE('',*,*,#2335,.F.);
#3277=ORIENTED_EDGE('',*,*,#2275,.F.);
#3278=ORIENTED_EDGE('',*,*,#2320,.F.);
#3279=ORIENTED_EDGE('',*,*,#2322,.F.);
#3280=ORIENTED_EDGE('',*,*,#2324,.F.);
#3281=ORIENTED_EDGE('',*,*,#2326,.F.);
#3282=ORIENTED_EDGE('',*,*,#2345,.F.);
#3283=ORIENTED_EDGE('',*,*,#2351,.F.);
#3284=ORIENTED_EDGE('',*,*,#2334,.T.);
#3285=ORIENTED_EDGE('',*,*,#2338,.T.);
#3286=ORIENTED_EDGE('',*,*,#2342,.T.);
#3287=ORIENTED_EDGE('',*,*,#2347,.T.);
#3288=ORIENTED_EDGE('',*,*,#2349,.T.);
#3289=ORIENTED_EDGE('',*,*,#2350,.T.);
#3290=ORIENTED_EDGE('',*,*,#2293,.T.);
#3291=ORIENTED_EDGE('',*,*,#2252,.F.);
#3292=ORIENTED_EDGE('',*,*,#2254,.F.);
#3293=ORIENTED_EDGE('',*,*,#2257,.F.);
#3294=ORIENTED_EDGE('',*,*,#2260,.F.);
#3295=ORIENTED_EDGE('',*,*,#2263,.F.);
#3296=ORIENTED_EDGE('',*,*,#2266,.F.);
#3297=ORIENTED_EDGE('',*,*,#2269,.F.);
#3298=ORIENTED_EDGE('',*,*,#2272,.F.);
#3299=ORIENTED_EDGE('',*,*,#2329,.T.);
#3300=ORIENTED_EDGE('',*,*,#2331,.T.);
#3301=ORIENTED_EDGE('',*,*,#2343,.T.);
#3302=ORIENTED_EDGE('',*,*,#2339,.T.);
#3303=ORIENTED_EDGE('',*,*,#2336,.T.);
#3304=ORIENTED_EDGE('',*,*,#2352,.T.);
#3305=ORIENTED_EDGE('',*,*,#2353,.F.);
#3306=ORIENTED_EDGE('',*,*,#2354,.T.);
#3307=ORIENTED_EDGE('',*,*,#2355,.F.);
#3308=ORIENTED_EDGE('',*,*,#2356,.T.);
#3309=ORIENTED_EDGE('',*,*,#2353,.T.);
#3310=ORIENTED_EDGE('',*,*,#2356,.F.);
#3311=ORIENTED_EDGE('',*,*,#2354,.F.);
#3312=ORIENTED_EDGE('',*,*,#2357,.T.);
#3313=ORIENTED_EDGE('',*,*,#2358,.F.);
#3314=ORIENTED_EDGE('',*,*,#2357,.F.);
#3315=ORIENTED_EDGE('',*,*,#2359,.F.);
#3316=ORIENTED_EDGE('',*,*,#2360,.T.);
#3317=ORIENTED_EDGE('',*,*,#2361,.F.);
#3318=ORIENTED_EDGE('',*,*,#2362,.T.);
#3319=ORIENTED_EDGE('',*,*,#2359,.T.);
#3320=ORIENTED_EDGE('',*,*,#2362,.F.);
#3321=ORIENTED_EDGE('',*,*,#2360,.F.);
#3322=ORIENTED_EDGE('',*,*,#2363,.T.);
#3323=ORIENTED_EDGE('',*,*,#2364,.F.);
#3324=ORIENTED_EDGE('',*,*,#2363,.F.);
#3325=ORIENTED_EDGE('',*,*,#2365,.T.);
#3326=ORIENTED_EDGE('',*,*,#2366,.T.);
#3327=ORIENTED_EDGE('',*,*,#2367,.T.);
#3328=ORIENTED_EDGE('',*,*,#2368,.T.);
#3329=ORIENTED_EDGE('',*,*,#2358,.T.);
#3330=ORIENTED_EDGE('',*,*,#2364,.T.);
#3331=ORIENTED_EDGE('',*,*,#2366,.F.);
#3332=ORIENTED_EDGE('',*,*,#2369,.T.);
#3333=ORIENTED_EDGE('',*,*,#2370,.F.);
#3334=ORIENTED_EDGE('',*,*,#2371,.F.);
#3335=ORIENTED_EDGE('',*,*,#2367,.F.);
#3336=ORIENTED_EDGE('',*,*,#2371,.T.);
#3337=ORIENTED_EDGE('',*,*,#2372,.F.);
#3338=ORIENTED_EDGE('',*,*,#2373,.F.);
#3339=ORIENTED_EDGE('',*,*,#2368,.F.);
#3340=ORIENTED_EDGE('',*,*,#2373,.T.);
#3341=ORIENTED_EDGE('',*,*,#2374,.F.);
#3342=ORIENTED_EDGE('',*,*,#2375,.F.);
#3343=ORIENTED_EDGE('',*,*,#2365,.F.);
#3344=ORIENTED_EDGE('',*,*,#2375,.T.);
#3345=ORIENTED_EDGE('',*,*,#2376,.F.);
#3346=ORIENTED_EDGE('',*,*,#2369,.F.);
#3347=ORIENTED_EDGE('',*,*,#2376,.T.);
#3348=ORIENTED_EDGE('',*,*,#2374,.T.);
#3349=ORIENTED_EDGE('',*,*,#2372,.T.);
#3350=ORIENTED_EDGE('',*,*,#2370,.T.);
#3351=ORIENTED_EDGE('',*,*,#2355,.T.);
#3352=ORIENTED_EDGE('',*,*,#2361,.T.);
#3353=ORIENTED_EDGE('',*,*,#2377,.T.);
#3354=ORIENTED_EDGE('',*,*,#2378,.T.);
#3355=ORIENTED_EDGE('',*,*,#2379,.T.);
#3356=ORIENTED_EDGE('',*,*,#2378,.F.);
#3357=ORIENTED_EDGE('',*,*,#2380,.T.);
#3358=ORIENTED_EDGE('',*,*,#2381,.F.);
#3359=ORIENTED_EDGE('',*,*,#2382,.T.);
#3360=ORIENTED_EDGE('',*,*,#2380,.F.);
#3361=ORIENTED_EDGE('',*,*,#2377,.F.);
#3362=ORIENTED_EDGE('',*,*,#2382,.F.);
#3363=ORIENTED_EDGE('',*,*,#2383,.T.);
#3364=ORIENTED_EDGE('',*,*,#2379,.F.);
#3365=ORIENTED_EDGE('',*,*,#2384,.F.);
#3366=ORIENTED_EDGE('',*,*,#2385,.T.);
#3367=ORIENTED_EDGE('',*,*,#2386,.T.);
#3368=ORIENTED_EDGE('',*,*,#2387,.F.);
#3369=ORIENTED_EDGE('',*,*,#2388,.F.);
#3370=ORIENTED_EDGE('',*,*,#2389,.T.);
#3371=ORIENTED_EDGE('',*,*,#2390,.T.);
#3372=ORIENTED_EDGE('',*,*,#2385,.F.);
#3373=ORIENTED_EDGE('',*,*,#2391,.F.);
#3374=ORIENTED_EDGE('',*,*,#2392,.T.);
#3375=ORIENTED_EDGE('',*,*,#2393,.T.);
#3376=ORIENTED_EDGE('',*,*,#2389,.F.);
#3377=ORIENTED_EDGE('',*,*,#2394,.F.);
#3378=ORIENTED_EDGE('',*,*,#2395,.T.);
#3379=ORIENTED_EDGE('',*,*,#2396,.T.);
#3380=ORIENTED_EDGE('',*,*,#2392,.F.);
#3381=ORIENTED_EDGE('',*,*,#2397,.F.);
#3382=ORIENTED_EDGE('',*,*,#2398,.T.);
#3383=ORIENTED_EDGE('',*,*,#2399,.T.);
#3384=ORIENTED_EDGE('',*,*,#2395,.F.);
#3385=ORIENTED_EDGE('',*,*,#2400,.F.);
#3386=ORIENTED_EDGE('',*,*,#2387,.T.);
#3387=ORIENTED_EDGE('',*,*,#2401,.T.);
#3388=ORIENTED_EDGE('',*,*,#2398,.F.);
#3389=ORIENTED_EDGE('',*,*,#2401,.F.);
#3390=ORIENTED_EDGE('',*,*,#2386,.F.);
#3391=ORIENTED_EDGE('',*,*,#2390,.F.);
#3392=ORIENTED_EDGE('',*,*,#2393,.F.);
#3393=ORIENTED_EDGE('',*,*,#2396,.F.);
#3394=ORIENTED_EDGE('',*,*,#2399,.F.);
#3395=ORIENTED_EDGE('',*,*,#2402,.T.);
#3396=ORIENTED_EDGE('',*,*,#2403,.T.);
#3397=ORIENTED_EDGE('',*,*,#2404,.T.);
#3398=ORIENTED_EDGE('',*,*,#2405,.T.);
#3399=ORIENTED_EDGE('',*,*,#2403,.F.);
#3400=ORIENTED_EDGE('',*,*,#2405,.F.);
#3401=ORIENTED_EDGE('',*,*,#2406,.T.);
#3402=ORIENTED_EDGE('',*,*,#2383,.F.);
#3403=ORIENTED_EDGE('',*,*,#2406,.F.);
#3404=ORIENTED_EDGE('',*,*,#2404,.F.);
#3405=ORIENTED_EDGE('',*,*,#2402,.F.);
#3406=ORIENTED_EDGE('',*,*,#2384,.T.);
#3407=ORIENTED_EDGE('',*,*,#2400,.T.);
#3408=ORIENTED_EDGE('',*,*,#2397,.T.);
#3409=ORIENTED_EDGE('',*,*,#2394,.T.);
#3410=ORIENTED_EDGE('',*,*,#2391,.T.);
#3411=ORIENTED_EDGE('',*,*,#2388,.T.);
#3412=ORIENTED_EDGE('',*,*,#2381,.T.);
#3413=ORIENTED_EDGE('',*,*,#2407,.F.);
#3414=ORIENTED_EDGE('',*,*,#2408,.T.);
#3415=ORIENTED_EDGE('',*,*,#2409,.F.);
#3416=ORIENTED_EDGE('',*,*,#2410,.F.);
#3417=ORIENTED_EDGE('',*,*,#2411,.F.);
#3418=ORIENTED_EDGE('',*,*,#2412,.F.);
#3419=ORIENTED_EDGE('',*,*,#2413,.F.);
#3420=ORIENTED_EDGE('',*,*,#2408,.F.);
#3421=ORIENTED_EDGE('',*,*,#2414,.F.);
#3422=ORIENTED_EDGE('',*,*,#2415,.F.);
#3423=ORIENTED_EDGE('',*,*,#2416,.F.);
#3424=ORIENTED_EDGE('',*,*,#2417,.F.);
#3425=ORIENTED_EDGE('',*,*,#2418,.F.);
#3426=ORIENTED_EDGE('',*,*,#2410,.T.);
#3427=ORIENTED_EDGE('',*,*,#2419,.F.);
#3428=ORIENTED_EDGE('',*,*,#2420,.F.);
#3429=ORIENTED_EDGE('',*,*,#2421,.F.);
#3430=ORIENTED_EDGE('',*,*,#2422,.F.);
#3431=ORIENTED_EDGE('',*,*,#2423,.F.);
#3432=ORIENTED_EDGE('',*,*,#2424,.T.);
#3433=ORIENTED_EDGE('',*,*,#2425,.F.);
#3434=ORIENTED_EDGE('',*,*,#2424,.F.);
#3435=ORIENTED_EDGE('',*,*,#2426,.F.);
#3436=ORIENTED_EDGE('',*,*,#2415,.T.);
#3437=ORIENTED_EDGE('',*,*,#2422,.T.);
#3438=ORIENTED_EDGE('',*,*,#2427,.T.);
#3439=ORIENTED_EDGE('',*,*,#2428,.T.);
#3440=ORIENTED_EDGE('',*,*,#2420,.T.);
#3441=ORIENTED_EDGE('',*,*,#2429,.T.);
#3442=ORIENTED_EDGE('',*,*,#2430,.T.);
#3443=ORIENTED_EDGE('',*,*,#2417,.T.);
#3444=ORIENTED_EDGE('',*,*,#2431,.T.);
#3445=ORIENTED_EDGE('',*,*,#2412,.T.);
#3446=ORIENTED_EDGE('',*,*,#2432,.T.);
#3447=ORIENTED_EDGE('',*,*,#2416,.T.);
#3448=ORIENTED_EDGE('',*,*,#2426,.T.);
#3449=ORIENTED_EDGE('',*,*,#2423,.T.);
#3450=ORIENTED_EDGE('',*,*,#2430,.F.);
#3451=ORIENTED_EDGE('',*,*,#2433,.T.);
#3452=ORIENTED_EDGE('',*,*,#2434,.T.);
#3453=ORIENTED_EDGE('',*,*,#2433,.F.);
#3454=ORIENTED_EDGE('',*,*,#2429,.F.);
#3455=ORIENTED_EDGE('',*,*,#2419,.T.);
#3456=ORIENTED_EDGE('',*,*,#2409,.T.);
#3457=ORIENTED_EDGE('',*,*,#2413,.T.);
#3458=ORIENTED_EDGE('',*,*,#2431,.F.);
#3459=ORIENTED_EDGE('',*,*,#2414,.T.);
#3460=ORIENTED_EDGE('',*,*,#2432,.F.);
#3461=ORIENTED_EDGE('',*,*,#2411,.T.);
#3462=ORIENTED_EDGE('',*,*,#2407,.T.);
#3463=ORIENTED_EDGE('',*,*,#2418,.T.);
#3464=ORIENTED_EDGE('',*,*,#2428,.F.);
#3465=ORIENTED_EDGE('',*,*,#2435,.T.);
#3466=ORIENTED_EDGE('',*,*,#2436,.F.);
#3467=ORIENTED_EDGE('',*,*,#2435,.F.);
#3468=ORIENTED_EDGE('',*,*,#2427,.F.);
#3469=ORIENTED_EDGE('',*,*,#2421,.T.);
#3470=ORIENTED_EDGE('',*,*,#2425,.T.);
#3471=ORIENTED_EDGE('',*,*,#2434,.F.);
#3472=ORIENTED_EDGE('',*,*,#2436,.T.);
#3473=ORIENTED_EDGE('',*,*,#2437,.F.);
#3474=ORIENTED_EDGE('',*,*,#2438,.T.);
#3475=ORIENTED_EDGE('',*,*,#2439,.T.);
#3476=ORIENTED_EDGE('',*,*,#2438,.F.);
#3477=ORIENTED_EDGE('',*,*,#2440,.F.);
#3478=ORIENTED_EDGE('',*,*,#2441,.T.);
#3479=ORIENTED_EDGE('',*,*,#2442,.F.);
#3480=ORIENTED_EDGE('',*,*,#2443,.F.);
#3481=ORIENTED_EDGE('',*,*,#2444,.F.);
#3482=ORIENTED_EDGE('',*,*,#2443,.T.);
#3483=ORIENTED_EDGE('',*,*,#2445,.F.);
#3484=ORIENTED_EDGE('',*,*,#2446,.F.);
#3485=ORIENTED_EDGE('',*,*,#2447,.T.);
#3486=ORIENTED_EDGE('',*,*,#2446,.T.);
#3487=ORIENTED_EDGE('',*,*,#2448,.F.);
#3488=ORIENTED_EDGE('',*,*,#2449,.F.);
#3489=ORIENTED_EDGE('',*,*,#2450,.T.);
#3490=ORIENTED_EDGE('',*,*,#2449,.T.);
#3491=ORIENTED_EDGE('',*,*,#2451,.F.);
#3492=ORIENTED_EDGE('',*,*,#2452,.F.);
#3493=ORIENTED_EDGE('',*,*,#2453,.T.);
#3494=ORIENTED_EDGE('',*,*,#2452,.T.);
#3495=ORIENTED_EDGE('',*,*,#2454,.F.);
#3496=ORIENTED_EDGE('',*,*,#2455,.F.);
#3497=ORIENTED_EDGE('',*,*,#2456,.T.);
#3498=ORIENTED_EDGE('',*,*,#2455,.T.);
#3499=ORIENTED_EDGE('',*,*,#2457,.F.);
#3500=ORIENTED_EDGE('',*,*,#2441,.F.);
#3501=ORIENTED_EDGE('',*,*,#2457,.T.);
#3502=ORIENTED_EDGE('',*,*,#2454,.T.);
#3503=ORIENTED_EDGE('',*,*,#2451,.T.);
#3504=ORIENTED_EDGE('',*,*,#2448,.T.);
#3505=ORIENTED_EDGE('',*,*,#2445,.T.);
#3506=ORIENTED_EDGE('',*,*,#2442,.T.);
#3507=ORIENTED_EDGE('',*,*,#2437,.T.);
#3508=ORIENTED_EDGE('',*,*,#2456,.F.);
#3509=ORIENTED_EDGE('',*,*,#2440,.T.);
#3510=ORIENTED_EDGE('',*,*,#2444,.T.);
#3511=ORIENTED_EDGE('',*,*,#2447,.F.);
#3512=ORIENTED_EDGE('',*,*,#2450,.F.);
#3513=ORIENTED_EDGE('',*,*,#2453,.F.);
#3514=ORIENTED_EDGE('',*,*,#2439,.F.);
#3515=ORIENTED_EDGE('',*,*,#2458,.F.);
#3516=ORIENTED_EDGE('',*,*,#2459,.F.);
#3517=ORIENTED_EDGE('',*,*,#2460,.T.);
#3518=ORIENTED_EDGE('',*,*,#2461,.F.);
#3519=ORIENTED_EDGE('',*,*,#2462,.F.);
#3520=ORIENTED_EDGE('',*,*,#2463,.F.);
#3521=ORIENTED_EDGE('',*,*,#2464,.T.);
#3522=ORIENTED_EDGE('',*,*,#2465,.F.);
#3523=ORIENTED_EDGE('',*,*,#2466,.F.);
#3524=ORIENTED_EDGE('',*,*,#2460,.F.);
#3525=ORIENTED_EDGE('',*,*,#2467,.F.);
#3526=ORIENTED_EDGE('',*,*,#2464,.F.);
#3527=ORIENTED_EDGE('',*,*,#2462,.T.);
#3528=ORIENTED_EDGE('',*,*,#2468,.F.);
#3529=ORIENTED_EDGE('',*,*,#2469,.F.);
#3530=ORIENTED_EDGE('',*,*,#2458,.T.);
#3531=ORIENTED_EDGE('',*,*,#2470,.F.);
#3532=ORIENTED_EDGE('',*,*,#2471,.F.);
#3533=ORIENTED_EDGE('',*,*,#2472,.T.);
#3534=ORIENTED_EDGE('',*,*,#2473,.F.);
#3535=ORIENTED_EDGE('',*,*,#2472,.F.);
#3536=ORIENTED_EDGE('',*,*,#2471,.T.);
#3537=ORIENTED_EDGE('',*,*,#2474,.F.);
#3538=ORIENTED_EDGE('',*,*,#2475,.T.);
#3539=ORIENTED_EDGE('',*,*,#2468,.T.);
#3540=ORIENTED_EDGE('',*,*,#2465,.T.);
#3541=ORIENTED_EDGE('',*,*,#2467,.T.);
#3542=ORIENTED_EDGE('',*,*,#2459,.T.);
#3543=ORIENTED_EDGE('',*,*,#2470,.T.);
#3544=ORIENTED_EDGE('',*,*,#2461,.T.);
#3545=ORIENTED_EDGE('',*,*,#2466,.T.);
#3546=ORIENTED_EDGE('',*,*,#2463,.T.);
#3547=ORIENTED_EDGE('',*,*,#2469,.T.);
#3548=ORIENTED_EDGE('',*,*,#2475,.F.);
#3549=ORIENTED_EDGE('',*,*,#2474,.T.);
#3550=ORIENTED_EDGE('',*,*,#2473,.T.);
#3551=ORIENTED_EDGE('',*,*,#2476,.T.);
#3552=ORIENTED_EDGE('',*,*,#2477,.T.);
#3553=ORIENTED_EDGE('',*,*,#2478,.T.);
#3554=ORIENTED_EDGE('',*,*,#2479,.T.);
#3555=ORIENTED_EDGE('',*,*,#2477,.F.);
#3556=ORIENTED_EDGE('',*,*,#2479,.F.);
#3557=ORIENTED_EDGE('',*,*,#2480,.T.);
#3558=ORIENTED_EDGE('',*,*,#2481,.T.);
#3559=ORIENTED_EDGE('',*,*,#2482,.T.);
#3560=ORIENTED_EDGE('',*,*,#2480,.F.);
#3561=ORIENTED_EDGE('',*,*,#2478,.F.);
#3562=ORIENTED_EDGE('',*,*,#2476,.F.);
#3563=ORIENTED_EDGE('',*,*,#2483,.F.);
#3564=ORIENTED_EDGE('',*,*,#2484,.F.);
#3565=ORIENTED_EDGE('',*,*,#2485,.T.);
#3566=ORIENTED_EDGE('',*,*,#2481,.F.);
#3567=ORIENTED_EDGE('',*,*,#2482,.F.);
#3568=ORIENTED_EDGE('',*,*,#2485,.F.);
#3569=ORIENTED_EDGE('',*,*,#2483,.T.);
#3570=ORIENTED_EDGE('',*,*,#2484,.T.);
#3571=ORIENTED_EDGE('',*,*,#2486,.T.);
#3572=ORIENTED_EDGE('',*,*,#2487,.T.);
#3573=ORIENTED_EDGE('',*,*,#2486,.F.);
#3574=ORIENTED_EDGE('',*,*,#2487,.F.);
#3575=ORIENTED_EDGE('',*,*,#2488,.T.);
#3576=ORIENTED_EDGE('',*,*,#2488,.F.);
#3577=ORIENTED_EDGE('',*,*,#2489,.T.);
#3578=ORIENTED_EDGE('',*,*,#2490,.F.);
#3579=ORIENTED_EDGE('',*,*,#2489,.F.);
#3580=ORIENTED_EDGE('',*,*,#2491,.F.);
#3581=ORIENTED_EDGE('',*,*,#2492,.T.);
#3582=ORIENTED_EDGE('',*,*,#2493,.F.);
#3583=ORIENTED_EDGE('',*,*,#2494,.T.);
#3584=ORIENTED_EDGE('',*,*,#2491,.T.);
#3585=ORIENTED_EDGE('',*,*,#2494,.F.);
#3586=ORIENTED_EDGE('',*,*,#2493,.T.);
#3587=ORIENTED_EDGE('',*,*,#2492,.F.);
#3588=ORIENTED_EDGE('',*,*,#2495,.T.);
#3589=ORIENTED_EDGE('',*,*,#2496,.F.);
#3590=ORIENTED_EDGE('',*,*,#2495,.F.);
#3591=ORIENTED_EDGE('',*,*,#2497,.F.);
#3592=ORIENTED_EDGE('',*,*,#2498,.T.);
#3593=ORIENTED_EDGE('',*,*,#2499,.F.);
#3594=ORIENTED_EDGE('',*,*,#2498,.F.);
#3595=ORIENTED_EDGE('',*,*,#2497,.T.);
#3596=ORIENTED_EDGE('',*,*,#2496,.T.);
#3597=ORIENTED_EDGE('',*,*,#2500,.F.);
#3598=ORIENTED_EDGE('',*,*,#2501,.T.);
#3599=ORIENTED_EDGE('',*,*,#2502,.T.);
#3600=ORIENTED_EDGE('',*,*,#2501,.F.);
#3601=ORIENTED_EDGE('',*,*,#2500,.T.);
#3602=ORIENTED_EDGE('',*,*,#2499,.T.);
#3603=ORIENTED_EDGE('',*,*,#2502,.F.);
#3604=ORIENTED_EDGE('',*,*,#2490,.T.);
#3605=ORIENTED_EDGE('',*,*,#2503,.F.);
#3606=ORIENTED_EDGE('',*,*,#2504,.T.);
#3607=ORIENTED_EDGE('',*,*,#2505,.F.);
#3608=ORIENTED_EDGE('',*,*,#2506,.F.);
#3609=ORIENTED_EDGE('',*,*,#2507,.T.);
#3610=ORIENTED_EDGE('',*,*,#2506,.T.);
#3611=ORIENTED_EDGE('',*,*,#2508,.F.);
#3612=ORIENTED_EDGE('',*,*,#2509,.F.);
#3613=ORIENTED_EDGE('',*,*,#2510,.T.);
#3614=ORIENTED_EDGE('',*,*,#2509,.T.);
#3615=ORIENTED_EDGE('',*,*,#2511,.F.);
#3616=ORIENTED_EDGE('',*,*,#2512,.F.);
#3617=ORIENTED_EDGE('',*,*,#2513,.T.);
#3618=ORIENTED_EDGE('',*,*,#2512,.T.);
#3619=ORIENTED_EDGE('',*,*,#2514,.F.);
#3620=ORIENTED_EDGE('',*,*,#2515,.F.);
#3621=ORIENTED_EDGE('',*,*,#2516,.T.);
#3622=ORIENTED_EDGE('',*,*,#2515,.T.);
#3623=ORIENTED_EDGE('',*,*,#2517,.F.);
#3624=ORIENTED_EDGE('',*,*,#2518,.F.);
#3625=ORIENTED_EDGE('',*,*,#2519,.T.);
#3626=ORIENTED_EDGE('',*,*,#2518,.T.);
#3627=ORIENTED_EDGE('',*,*,#2520,.F.);
#3628=ORIENTED_EDGE('',*,*,#2521,.F.);
#3629=ORIENTED_EDGE('',*,*,#2522,.T.);
#3630=ORIENTED_EDGE('',*,*,#2521,.T.);
#3631=ORIENTED_EDGE('',*,*,#2523,.F.);
#3632=ORIENTED_EDGE('',*,*,#2524,.F.);
#3633=ORIENTED_EDGE('',*,*,#2525,.T.);
#3634=ORIENTED_EDGE('',*,*,#2524,.T.);
#3635=ORIENTED_EDGE('',*,*,#2526,.F.);
#3636=ORIENTED_EDGE('',*,*,#2504,.F.);
#3637=ORIENTED_EDGE('',*,*,#2526,.T.);
#3638=ORIENTED_EDGE('',*,*,#2523,.T.);
#3639=ORIENTED_EDGE('',*,*,#2520,.T.);
#3640=ORIENTED_EDGE('',*,*,#2517,.T.);
#3641=ORIENTED_EDGE('',*,*,#2514,.T.);
#3642=ORIENTED_EDGE('',*,*,#2511,.T.);
#3643=ORIENTED_EDGE('',*,*,#2508,.T.);
#3644=ORIENTED_EDGE('',*,*,#2505,.T.);
#3645=ORIENTED_EDGE('',*,*,#2525,.F.);
#3646=ORIENTED_EDGE('',*,*,#2503,.T.);
#3647=ORIENTED_EDGE('',*,*,#2507,.F.);
#3648=ORIENTED_EDGE('',*,*,#2510,.F.);
#3649=ORIENTED_EDGE('',*,*,#2513,.F.);
#3650=ORIENTED_EDGE('',*,*,#2516,.F.);
#3651=ORIENTED_EDGE('',*,*,#2519,.F.);
#3652=ORIENTED_EDGE('',*,*,#2522,.F.);
#3653=PLANE('',#4113);
#3654=PLANE('',#4114);
#3655=PLANE('',#4115);
#3656=PLANE('',#4116);
#3657=PLANE('',#4117);
#3658=PLANE('',#4118);
#3659=PLANE('',#4119);
#3660=PLANE('',#4120);
#3661=PLANE('',#4121);
#3662=PLANE('',#4124);
#3663=PLANE('',#4125);
#3664=PLANE('',#4128);
#3665=PLANE('',#4154);
#3666=PLANE('',#4157);
#3667=PLANE('',#4175);
#3668=PLANE('',#4189);
#3669=PLANE('',#4190);
#3670=PLANE('',#4205);
#3671=PLANE('',#4206);
#3672=PLANE('',#4239);
#3673=PLANE('',#4242);
#3674=PLANE('',#4249);
#3675=PLANE('',#4252);
#3676=PLANE('',#4257);
#3677=PLANE('',#4261);
#3678=PLANE('',#4272);
#3679=PLANE('',#4279);
#3680=PLANE('',#4280);
#3681=PLANE('',#4282);
#3682=PLANE('',#4283);
#3683=PLANE('',#4288);
#3684=PLANE('',#4292);
#3685=PLANE('',#4293);
#3686=PLANE('',#4297);
#3687=PLANE('',#4298);
#3688=PLANE('',#4301);
#3689=PLANE('',#4305);
#3690=PLANE('',#4308);
#3691=PLANE('',#4310);
#3692=PLANE('',#4311);
#3693=PLANE('',#4312);
#3694=PLANE('',#4313);
#3695=PLANE('',#4314);
#3696=PLANE('',#4318);
#3697=PLANE('',#4322);
#3698=PLANE('',#4323);
#3699=PLANE('',#4324);
#3700=PLANE('',#4325);
#3701=PLANE('',#4326);
#3702=PLANE('',#4334);
#3703=PLANE('',#4335);
#3704=PLANE('',#4336);
#3705=PLANE('',#4337);
#3706=PLANE('',#4338);
#3707=PLANE('',#4339);
#3708=PLANE('',#4340);
#3709=PLANE('',#4341);
#3710=PLANE('',#4342);
#3711=PLANE('',#4343);
#3712=PLANE('',#4345);
#3713=PLANE('',#4352);
#3714=PLANE('',#4359);
#3715=PLANE('',#4360);
#3716=PLANE('',#4361);
#3717=PLANE('',#4362);
#3718=PLANE('',#4363);
#3719=PLANE('',#4364);
#3720=PLANE('',#4373);
#3721=PLANE('',#4375);
#3722=PLANE('',#4376);
#3723=PLANE('',#4377);
#3724=PLANE('',#4378);
#3725=PLANE('',#4379);
#3726=PLANE('',#4380);
#3727=PLANE('',#4381);
#3728=PLANE('',#4388);
#3729=PLANE('',#4389);
#3730=PLANE('',#4391);
#3731=PLANE('',#4394);
#3732=PLANE('',#4395);
#3733=PLANE('',#4396);
#3734=PLANE('',#4397);
#3735=PLANE('',#4398);
#3736=PLANE('',#4401);
#3737=PLANE('',#4406);
#3738=PLANE('',#4413);
#3739=PLANE('',#4421);
#3740=PLANE('',#4431);
#3741=PLANE('',#4432);
#3742=PLANE('',#4433);
#3743=PLANE('',#4435);
#3744=PLANE('',#4436);
#3745=PLANE('',#4437);
#3746=PLANE('',#4440);
#3747=PLANE('',#4443);
#3748=PLANE('',#4448);
#3749=PLANE('',#4451);
#3750=PLANE('',#4461);
#3751=PLANE('',#4468);
#3752=PLANE('',#4472);
#3753=PLANE('',#4477);
#3754=PLANE('',#4483);
#3755=PLANE('',#4487);
#3756=PLANE('',#4488);
#3757=PLANE('',#4490);
#3758=PLANE('',#4491);
#3759=PLANE('',#4492);
#3760=PLANE('',#4493);
#3761=PLANE('',#4494);
#3762=PLANE('',#4495);
#3763=PLANE('',#4496);
#3764=PLANE('',#4497);
#3765=PLANE('',#4498);
#3766=PLANE('',#4499);
#3767=ADVANCED_FACE('',(#526),#3653,.F.);
#3768=ADVANCED_FACE('',(#527),#3654,.F.);
#3769=ADVANCED_FACE('',(#528),#3655,.F.);
#3770=ADVANCED_FACE('',(#529),#3656,.F.);
#3771=ADVANCED_FACE('',(#530),#3657,.F.);
#3772=ADVANCED_FACE('',(#531),#3658,.F.);
#3773=ADVANCED_FACE('',(#532),#3659,.F.);
#3774=ADVANCED_FACE('',(#533),#3660,.F.);
#3775=ADVANCED_FACE('',(#534,#337,#338),#3661,.T.);
#3776=ADVANCED_FACE('',(#535),#3662,.T.);
#3777=ADVANCED_FACE('',(#536),#3663,.T.);
#3778=ADVANCED_FACE('',(#537,#339,#340),#3664,.T.);
#3779=ADVANCED_FACE('',(#538),#300,.F.);
#3780=ADVANCED_FACE('',(#539),#193,.T.);
#3781=ADVANCED_FACE('',(#540),#301,.F.);
#3782=ADVANCED_FACE('',(#541),#302,.F.);
#3783=ADVANCED_FACE('',(#542),#194,.T.);
#3784=ADVANCED_FACE('',(#543),#104,.T.);
#3785=ADVANCED_FACE('',(#544),#195,.T.);
#3786=ADVANCED_FACE('',(#545),#105,.F.);
#3787=ADVANCED_FACE('',(#546,#341),#3665,.T.);
#3788=ADVANCED_FACE('',(#547),#106,.F.);
#3789=ADVANCED_FACE('',(#548),#3666,.T.);
#3790=ADVANCED_FACE('',(#549),#196,.T.);
#3791=ADVANCED_FACE('',(#550),#107,.T.);
#3792=ADVANCED_FACE('',(#551),#303,.F.);
#3793=ADVANCED_FACE('',(#552),#197,.T.);
#3794=ADVANCED_FACE('',(#553),#304,.F.);
#3795=ADVANCED_FACE('',(#554),#305,.F.);
#3796=ADVANCED_FACE('',(#555),#198,.T.);
#3797=ADVANCED_FACE('',(#556,#342),#3667,.T.);
#3798=ADVANCED_FACE('',(#557),#108,.F.);
#3799=ADVANCED_FACE('',(#558),#109,.T.);
#3800=ADVANCED_FACE('',(#559),#306,.F.);
#3801=ADVANCED_FACE('',(#560),#307,.F.);
#3802=ADVANCED_FACE('',(#561),#199,.T.);
#3803=ADVANCED_FACE('',(#562),#308,.F.);
#3804=ADVANCED_FACE('',(#563),#110,.T.);
#3805=ADVANCED_FACE('',(#564),#3668,.T.);
#3806=ADVANCED_FACE('',(#565),#3669,.T.);
#3807=ADVANCED_FACE('',(#566),#309,.F.);
#3808=ADVANCED_FACE('',(#567),#200,.T.);
#3809=ADVANCED_FACE('',(#568),#310,.F.);
#3810=ADVANCED_FACE('',(#569),#311,.F.);
#3811=ADVANCED_FACE('',(#570),#312,.F.);
#3812=ADVANCED_FACE('',(#571),#111,.F.);
#3813=ADVANCED_FACE('',(#572),#112,.F.);
#3814=ADVANCED_FACE('',(#573),#3670,.T.);
#3815=ADVANCED_FACE('',(#574,#343),#3671,.T.);
#3816=ADVANCED_FACE('',(#575),#313,.F.);
#3817=ADVANCED_FACE('',(#576),#113,.T.);
#3818=ADVANCED_FACE('',(#577),#201,.T.);
#3819=ADVANCED_FACE('',(#578),#114,.T.);
#3820=ADVANCED_FACE('',(#579),#314,.F.);
#3821=ADVANCED_FACE('',(#580),#315,.F.);
#3822=ADVANCED_FACE('',(#581),#316,.F.);
#3823=ADVANCED_FACE('',(#582),#202,.T.);
#3824=ADVANCED_FACE('',(#583),#115,.T.);
#3825=ADVANCED_FACE('',(#584),#116,.T.);
#3826=ADVANCED_FACE('',(#585),#102,.T.);
#3827=ADVANCED_FACE('',(#586),#103,.T.);
#3828=ADVANCED_FACE('',(#587),#117,.T.);
#3829=ADVANCED_FACE('',(#588),#3672,.F.);
#3830=ADVANCED_FACE('',(#589),#118,.T.);
#3831=ADVANCED_FACE('',(#590),#3673,.F.);
#3832=ADVANCED_FACE('',(#591),#119,.F.);
#3833=ADVANCED_FACE('',(#592),#120,.T.);
#3834=ADVANCED_FACE('',(#593),#121,.F.);
#3835=ADVANCED_FACE('',(#594),#3674,.F.);
#3836=ADVANCED_FACE('',(#595),#122,.T.);
#3837=ADVANCED_FACE('',(#596,#344),#3675,.T.);
#3838=ADVANCED_FACE('',(#597),#123,.F.);
#3839=ADVANCED_FACE('',(#598),#3676,.T.);
#3840=ADVANCED_FACE('',(#599),#124,.F.);
#3841=ADVANCED_FACE('',(#600),#125,.F.);
#3842=ADVANCED_FACE('',(#601,#345),#3677,.T.);
#3843=ADVANCED_FACE('',(#602),#126,.F.);
#3844=ADVANCED_FACE('',(#603),#127,.F.);
#3845=ADVANCED_FACE('',(#604),#128,.T.);
#3846=ADVANCED_FACE('',(#605),#129,.F.);
#3847=ADVANCED_FACE('',(#606),#130,.F.);
#3848=ADVANCED_FACE('',(#607),#131,.F.);
#3849=ADVANCED_FACE('',(#608),#3678,.T.);
#3850=ADVANCED_FACE('',(#609),#99,.F.);
#3851=ADVANCED_FACE('',(#610),#132,.F.);
#3852=ADVANCED_FACE('',(#611),#100,.F.);
#3853=ADVANCED_FACE('',(#612),#133,.F.);
#3854=ADVANCED_FACE('',(#613),#3679,.T.);
#3855=ADVANCED_FACE('',(#614),#3680,.T.);
#3856=ADVANCED_FACE('',(#615),#134,.T.);
#3857=ADVANCED_FACE('',(#616,#346,#347),#3681,.T.);
#3858=ADVANCED_FACE('',(#617),#3682,.T.);
#3859=ADVANCED_FACE('',(#618),#135,.F.);
#3860=ADVANCED_FACE('',(#619),#3683,.T.);
#3861=ADVANCED_FACE('',(#620),#136,.F.);
#3862=ADVANCED_FACE('',(#621),#3684,.T.);
#3863=ADVANCED_FACE('',(#622),#317,.T.);
#3864=ADVANCED_FACE('',(#623),#318,.T.);
#3865=ADVANCED_FACE('',(#624),#319,.T.);
#3866=ADVANCED_FACE('',(#625),#320,.T.);
#3867=ADVANCED_FACE('',(#626),#321,.T.);
#3868=ADVANCED_FACE('',(#627),#322,.T.);
#3869=ADVANCED_FACE('',(#628),#323,.T.);
#3870=ADVANCED_FACE('',(#629),#324,.T.);
#3871=ADVANCED_FACE('',(#630),#325,.T.);
#3872=ADVANCED_FACE('',(#631),#326,.T.);
#3873=ADVANCED_FACE('',(#632),#327,.T.);
#3874=ADVANCED_FACE('',(#633),#3685,.F.);
#3875=ADVANCED_FACE('',(#634),#137,.T.);
#3876=ADVANCED_FACE('',(#635),#3686,.F.);
#3877=ADVANCED_FACE('',(#636),#328,.T.);
#3878=ADVANCED_FACE('',(#637),#329,.T.);
#3879=ADVANCED_FACE('',(#638),#330,.T.);
#3880=ADVANCED_FACE('',(#639),#331,.T.);
#3881=ADVANCED_FACE('',(#640),#332,.T.);
#3882=ADVANCED_FACE('',(#641),#333,.T.);
#3883=ADVANCED_FACE('',(#642),#334,.T.);
#3884=ADVANCED_FACE('',(#643),#335,.T.);
#3885=ADVANCED_FACE('',(#644),#336,.T.);
#3886=ADVANCED_FACE('',(#645),#3687,.T.);
#3887=ADVANCED_FACE('',(#646),#138,.T.);
#3888=ADVANCED_FACE('',(#647),#3688,.T.);
#3889=ADVANCED_FACE('',(#648),#139,.F.);
#3890=ADVANCED_FACE('',(#649),#140,.T.);
#3891=ADVANCED_FACE('',(#650),#141,.F.);
#3892=ADVANCED_FACE('',(#651),#3689,.T.);
#3893=ADVANCED_FACE('',(#652),#142,.T.);
#3894=ADVANCED_FACE('',(#653),#3690,.T.);
#3895=ADVANCED_FACE('',(#654),#3691,.T.);
#3896=ADVANCED_FACE('',(#655),#3692,.T.);
#3897=ADVANCED_FACE('',(#656),#3693,.T.);
#3898=ADVANCED_FACE('',(#657),#3694,.T.);
#3899=ADVANCED_FACE('',(#658,#348,#349),#3695,.F.);
#3900=ADVANCED_FACE('',(#659),#143,.F.);
#3901=ADVANCED_FACE('',(#660),#3696,.F.);
#3902=ADVANCED_FACE('',(#661),#144,.T.);
#3903=ADVANCED_FACE('',(#662),#3697,.F.);
#3904=ADVANCED_FACE('',(#663),#3698,.T.);
#3905=ADVANCED_FACE('',(#664),#3699,.T.);
#3906=ADVANCED_FACE('',(#665),#3700,.T.);
#3907=ADVANCED_FACE('',(#666),#3701,.T.);
#3908=ADVANCED_FACE('',(#667),#101,.F.);
#3909=ADVANCED_FACE('',(#668),#145,.F.);
#3910=ADVANCED_FACE('',(#669),#146,.F.);
#3911=ADVANCED_FACE('',(#670),#3702,.F.);
#3912=ADVANCED_FACE('',(#671),#3703,.T.);
#3913=ADVANCED_FACE('',(#672),#3704,.T.);
#3914=ADVANCED_FACE('',(#673),#3705,.T.);
#3915=ADVANCED_FACE('',(#674),#3706,.T.);
#3916=ADVANCED_FACE('',(#675),#3707,.T.);
#3917=ADVANCED_FACE('',(#676),#3708,.T.);
#3918=ADVANCED_FACE('',(#677),#3709,.T.);
#3919=ADVANCED_FACE('',(#678,#350,#351),#3710,.T.);
#3920=ADVANCED_FACE('',(#679),#3711,.F.);
#3921=ADVANCED_FACE('',(#680,#352),#3712,.F.);
#3922=ADVANCED_FACE('',(#681),#147,.F.);
#3923=ADVANCED_FACE('',(#682),#148,.F.);
#3924=ADVANCED_FACE('',(#683,#353),#3713,.F.);
#3925=ADVANCED_FACE('',(#684),#149,.F.);
#3926=ADVANCED_FACE('',(#685),#150,.F.);
#3927=ADVANCED_FACE('',(#686,#354,#355),#3714,.F.);
#3928=ADVANCED_FACE('',(#687),#3715,.T.);
#3929=ADVANCED_FACE('',(#688),#3716,.T.);
#3930=ADVANCED_FACE('',(#689),#3717,.T.);
#3931=ADVANCED_FACE('',(#690),#3718,.T.);
#3932=ADVANCED_FACE('',(#691,#356,#357),#3719,.T.);
#3933=ADVANCED_FACE('',(#692),#203,.F.);
#3934=ADVANCED_FACE('',(#693),#151,.T.);
#3935=ADVANCED_FACE('',(#694,#358),#3720,.T.);
#3936=ADVANCED_FACE('',(#695),#3721,.F.);
#3937=ADVANCED_FACE('',(#696),#3722,.F.);
#3938=ADVANCED_FACE('',(#697),#3723,.F.);
#3939=ADVANCED_FACE('',(#698),#3724,.F.);
#3940=ADVANCED_FACE('',(#699),#3725,.F.);
#3941=ADVANCED_FACE('',(#700),#3726,.F.);
#3942=ADVANCED_FACE('',(#701),#3727,.F.);
#3943=ADVANCED_FACE('',(#702),#204,.T.);
#3944=ADVANCED_FACE('',(#703),#152,.T.);
#3945=ADVANCED_FACE('',(#704,#359),#3728,.F.);
#3946=ADVANCED_FACE('',(#705),#3729,.T.);
#3947=ADVANCED_FACE('',(#706),#3730,.F.);
#3948=ADVANCED_FACE('',(#707),#3731,.F.);
#3949=ADVANCED_FACE('',(#708),#3732,.F.);
#3950=ADVANCED_FACE('',(#709),#3733,.F.);
#3951=ADVANCED_FACE('',(#710),#3734,.F.);
#3952=ADVANCED_FACE('',(#711),#3735,.F.);
#3953=ADVANCED_FACE('',(#712),#3736,.T.);
#3954=ADVANCED_FACE('',(#713),#3737,.T.);
#3955=ADVANCED_FACE('',(#714),#153,.T.);
#3956=ADVANCED_FACE('',(#715),#154,.F.);
#3957=ADVANCED_FACE('',(#716,#360),#3738,.F.);
#3958=ADVANCED_FACE('',(#717),#155,.F.);
#3959=ADVANCED_FACE('',(#718),#156,.F.);
#3960=ADVANCED_FACE('',(#719),#3739,.T.);
#3961=ADVANCED_FACE('',(#720),#157,.T.);
#3962=ADVANCED_FACE('',(#721),#158,.T.);
#3963=ADVANCED_FACE('',(#722),#159,.T.);
#3964=ADVANCED_FACE('',(#723),#3740,.T.);
#3965=ADVANCED_FACE('',(#724,#361),#3741,.T.);
#3966=ADVANCED_FACE('',(#725,#362),#3742,.F.);
#3967=ADVANCED_FACE('',(#726),#3743,.F.);
#3968=ADVANCED_FACE('',(#727),#3744,.F.);
#3969=ADVANCED_FACE('',(#728),#3745,.T.);
#3970=ADVANCED_FACE('',(#729),#3746,.F.);
#3971=ADVANCED_FACE('',(#730),#3747,.F.);
#3972=ADVANCED_FACE('',(#731),#160,.T.);
#3973=ADVANCED_FACE('',(#732),#3748,.T.);
#3974=ADVANCED_FACE('',(#733),#161,.T.);
#3975=ADVANCED_FACE('',(#734,#363),#3749,.T.);
#3976=ADVANCED_FACE('',(#735),#205,.T.);
#3977=ADVANCED_FACE('',(#736),#162,.T.);
#3978=ADVANCED_FACE('',(#737),#3750,.T.);
#3979=ADVANCED_FACE('',(#738),#206,.F.);
#3980=ADVANCED_FACE('',(#739),#163,.T.);
#3981=ADVANCED_FACE('',(#740,#364),#3751,.F.);
#3982=ADVANCED_FACE('',(#741),#164,.T.);
#3983=ADVANCED_FACE('',(#742,#365),#3752,.F.);
#3984=ADVANCED_FACE('',(#743),#165,.T.);
#3985=ADVANCED_FACE('',(#744),#3753,.T.);
#3986=ADVANCED_FACE('',(#745),#166,.T.);
#3987=ADVANCED_FACE('',(#746),#167,.T.);
#3988=ADVANCED_FACE('',(#747,#366),#3754,.T.);
#3989=ADVANCED_FACE('',(#748),#168,.T.);
#3990=ADVANCED_FACE('',(#749,#367),#3755,.T.);
#3991=ADVANCED_FACE('',(#750,#368),#3756,.F.);
#3992=ADVANCED_FACE('',(#751),#3757,.T.);
#3993=ADVANCED_FACE('',(#752),#3758,.T.);
#3994=ADVANCED_FACE('',(#753),#3759,.T.);
#3995=ADVANCED_FACE('',(#754),#3760,.T.);
#3996=ADVANCED_FACE('',(#755),#3761,.T.);
#3997=ADVANCED_FACE('',(#756),#3762,.T.);
#3998=ADVANCED_FACE('',(#757),#3763,.T.);
#3999=ADVANCED_FACE('',(#758),#3764,.T.);
#4000=ADVANCED_FACE('',(#759),#3765,.T.);
#4001=ADVANCED_FACE('',(#760),#3766,.F.);
#4002=CLOSED_SHELL('',(#3767,#3768,#3769,#3770,#3771,#3772,#3773,#3774,
#3775,#3776,#3777,#3778,#3779,#3780,#3781,#3782,#3783,#3784,#3785,#3786,
#3787,#3788,#3789,#3790,#3791,#3792,#3793,#3794,#3795,#3796,#3797,#3798,
#3799,#3800,#3801,#3802,#3803,#3804,#3805,#3806,#3807,#3808,#3809,#3810,
#3811,#3812,#3813,#3814,#3815,#3816,#3817,#3818,#3819,#3820,#3821,#3822,
#3823,#3824,#3825,#3826,#3827,#3828,#3829,#3830,#3831,#3832,#3833,#3834,
#3835,#3836,#3837,#3838,#3839,#3840,#3841,#3842,#3843,#3844,#3845,#3846,
#3847,#3848,#3849,#3850,#3851,#3852,#3853,#3854,#3855,#3856,#3857,#3858));
#4003=CLOSED_SHELL('',(#3859,#3860,#3861,#3862,#3863,#3864,#3865,#3866,
#3867,#3868,#3869,#3870,#3871,#3872,#3873,#3874,#3875,#3876,#3877,#3878,
#3879,#3880,#3881,#3882,#3883,#3884,#3885,#3886,#3887,#3888,#3889,#3890,
#3891,#3892,#3893,#3894,#3895,#3896,#3897,#3898,#3899,#3900,#3901,#3902,
#3903,#3904,#3905,#3906,#3907,#3908,#3909,#3910,#3911,#3912,#3913,#3914,
#3915,#3916,#3917,#3918,#3919,#3920));
#4004=CLOSED_SHELL('',(#3921,#3922,#3923,#3924,#3925,#3926,#3927,#3928,
#3929,#3930,#3931,#3932));
#4005=CLOSED_SHELL('',(#3933,#3934,#3935,#3936,#3937,#3938,#3939,#3940,
#3941,#3942,#3943,#3944,#3945,#3946));
#4006=CLOSED_SHELL('',(#3947,#3948,#3949,#3950,#3951,#3952,#3953,#3954,
#3955,#3956,#3957));
#4007=CLOSED_SHELL('',(#3958,#3959,#3960,#3961,#3962,#3963,#3964,#3965,
#3966));
#4008=CLOSED_SHELL('',(#3967,#3968,#3969,#3970,#3971,#3972,#3973,#3974,
#3975));
#4009=CLOSED_SHELL('',(#3976,#3977,#3978,#3979,#3980,#3981,#3982,#3983,
#3984,#3985,#3986,#3987,#3988,#3989,#3990,#3991));
#4010=CLOSED_SHELL('',(#3992,#3993,#3994,#3995,#3996,#3997,#3998,#3999,
#4000,#4001));
#4011=DERIVED_UNIT_ELEMENT(#4029,1.);
#4012=DERIVED_UNIT_ELEMENT(#8447,-3.);
#4013=DERIVED_UNIT_ELEMENT(#4029,1.);
#4014=DERIVED_UNIT_ELEMENT(#8447,-3.);
#4015=DERIVED_UNIT_ELEMENT(#4029,1.);
#4016=DERIVED_UNIT_ELEMENT(#8447,-3.);
#4017=DERIVED_UNIT_ELEMENT(#4029,1.);
#4018=DERIVED_UNIT_ELEMENT(#8447,-3.);
#4019=DERIVED_UNIT_ELEMENT(#4029,1.);
#4020=DERIVED_UNIT_ELEMENT(#8447,-3.);
#4021=DERIVED_UNIT_ELEMENT(#4029,1.);
#4022=DERIVED_UNIT_ELEMENT(#8447,-3.);
#4023=DERIVED_UNIT_ELEMENT(#4029,1.);
#4024=DERIVED_UNIT_ELEMENT(#8447,-3.);
#4025=DERIVED_UNIT_ELEMENT(#4029,1.);
#4026=DERIVED_UNIT_ELEMENT(#8447,-3.);
#4027=DERIVED_UNIT_ELEMENT(#4029,1.);
#4028=DERIVED_UNIT_ELEMENT(#8447,-3.);
#4029=(
MASS_UNIT()
NAMED_UNIT(*)
SI_UNIT(.KILO.,.GRAM.)
);
#4030=DERIVED_UNIT((#4011,#4012));
#4031=DERIVED_UNIT((#4013,#4014));
#4032=DERIVED_UNIT((#4015,#4016));
#4033=DERIVED_UNIT((#4017,#4018));
#4034=DERIVED_UNIT((#4019,#4020));
#4035=DERIVED_UNIT((#4021,#4022));
#4036=DERIVED_UNIT((#4023,#4024));
#4037=DERIVED_UNIT((#4025,#4026));
#4038=DERIVED_UNIT((#4027,#4028));
#4039=MEASURE_REPRESENTATION_ITEM('density measure',
POSITIVE_RATIO_MEASURE(7850.),#4030);
#4040=MEASURE_REPRESENTATION_ITEM('density measure',
POSITIVE_RATIO_MEASURE(7850.),#4031);
#4041=MEASURE_REPRESENTATION_ITEM('density measure',
POSITIVE_RATIO_MEASURE(7850.),#4032);
#4042=MEASURE_REPRESENTATION_ITEM('density measure',
POSITIVE_RATIO_MEASURE(7850.),#4033);
#4043=MEASURE_REPRESENTATION_ITEM('density measure',
POSITIVE_RATIO_MEASURE(7850.),#4034);
#4044=MEASURE_REPRESENTATION_ITEM('density measure',
POSITIVE_RATIO_MEASURE(7850.),#4035);
#4045=MEASURE_REPRESENTATION_ITEM('density measure',
POSITIVE_RATIO_MEASURE(7850.),#4036);
#4046=MEASURE_REPRESENTATION_ITEM('density measure',
POSITIVE_RATIO_MEASURE(7850.),#4037);
#4047=MEASURE_REPRESENTATION_ITEM('density measure',
POSITIVE_RATIO_MEASURE(7850.),#4038);
#4048=PROPERTY_DEFINITION_REPRESENTATION(#4093,#4066);
#4049=PROPERTY_DEFINITION_REPRESENTATION(#4094,#4067);
#4050=PROPERTY_DEFINITION_REPRESENTATION(#4095,#4068);
#4051=PROPERTY_DEFINITION_REPRESENTATION(#4096,#4069);
#4052=PROPERTY_DEFINITION_REPRESENTATION(#4097,#4070);
#4053=PROPERTY_DEFINITION_REPRESENTATION(#4098,#4071);
#4054=PROPERTY_DEFINITION_REPRESENTATION(#4099,#4072);
#4055=PROPERTY_DEFINITION_REPRESENTATION(#4100,#4073);
#4056=PROPERTY_DEFINITION_REPRESENTATION(#4101,#4074);
#4057=PROPERTY_DEFINITION_REPRESENTATION(#4102,#4075);
#4058=PROPERTY_DEFINITION_REPRESENTATION(#4103,#4076);
#4059=PROPERTY_DEFINITION_REPRESENTATION(#4104,#4077);
#4060=PROPERTY_DEFINITION_REPRESENTATION(#4105,#4078);
#4061=PROPERTY_DEFINITION_REPRESENTATION(#4106,#4079);
#4062=PROPERTY_DEFINITION_REPRESENTATION(#4107,#4080);
#4063=PROPERTY_DEFINITION_REPRESENTATION(#4108,#4081);
#4064=PROPERTY_DEFINITION_REPRESENTATION(#4109,#4082);
#4065=PROPERTY_DEFINITION_REPRESENTATION(#4110,#4083);
#4066=REPRESENTATION('material name',(#4084),#8436);
#4067=REPRESENTATION('density',(#4039),#8436);
#4068=REPRESENTATION('material name',(#4085),#8437);
#4069=REPRESENTATION('density',(#4040),#8437);
#4070=REPRESENTATION('material name',(#4086),#8438);
#4071=REPRESENTATION('density',(#4041),#8438);
#4072=REPRESENTATION('material name',(#4087),#8439);
#4073=REPRESENTATION('density',(#4042),#8439);
#4074=REPRESENTATION('material name',(#4088),#8440);
#4075=REPRESENTATION('density',(#4043),#8440);
#4076=REPRESENTATION('material name',(#4089),#8441);
#4077=REPRESENTATION('density',(#4044),#8441);
#4078=REPRESENTATION('material name',(#4090),#8442);
#4079=REPRESENTATION('density',(#4045),#8442);
#4080=REPRESENTATION('material name',(#4091),#8443);
#4081=REPRESENTATION('density',(#4046),#8443);
#4082=REPRESENTATION('material name',(#4092),#8444);
#4083=REPRESENTATION('density',(#4047),#8444);
#4084=DESCRIPTIVE_REPRESENTATION_ITEM('Steel','Steel');
#4085=DESCRIPTIVE_REPRESENTATION_ITEM('Steel','Steel');
#4086=DESCRIPTIVE_REPRESENTATION_ITEM('Steel','Steel');
#4087=DESCRIPTIVE_REPRESENTATION_ITEM('Steel','Steel');
#4088=DESCRIPTIVE_REPRESENTATION_ITEM('Steel','Steel');
#4089=DESCRIPTIVE_REPRESENTATION_ITEM('Steel','Steel');
#4090=DESCRIPTIVE_REPRESENTATION_ITEM('Steel','Steel');
#4091=DESCRIPTIVE_REPRESENTATION_ITEM('Steel','Steel');
#4092=DESCRIPTIVE_REPRESENTATION_ITEM('Steel','Steel');
#4093=PROPERTY_DEFINITION('material property','material name',#8495);
#4094=PROPERTY_DEFINITION('material property','density of part',#8495);
#4095=PROPERTY_DEFINITION('material property','material name',#8496);
#4096=PROPERTY_DEFINITION('material property','density of part',#8496);
#4097=PROPERTY_DEFINITION('material property','material name',#8497);
#4098=PROPERTY_DEFINITION('material property','density of part',#8497);
#4099=PROPERTY_DEFINITION('material property','material name',#8498);
#4100=PROPERTY_DEFINITION('material property','density of part',#8498);
#4101=PROPERTY_DEFINITION('material property','material name',#8499);
#4102=PROPERTY_DEFINITION('material property','density of part',#8499);
#4103=PROPERTY_DEFINITION('material property','material name',#8500);
#4104=PROPERTY_DEFINITION('material property','density of part',#8500);
#4105=PROPERTY_DEFINITION('material property','material name',#8501);
#4106=PROPERTY_DEFINITION('material property','density of part',#8501);
#4107=PROPERTY_DEFINITION('material property','material name',#8502);
#4108=PROPERTY_DEFINITION('material property','density of part',#8502);
#4109=PROPERTY_DEFINITION('material property','material name',#8503);
#4110=PROPERTY_DEFINITION('material property','density of part',#8503);
#4111=AXIS2_PLACEMENT_3D('',#5606,#4513,#4514);
#4112=AXIS2_PLACEMENT_3D('',#5607,#4515,#4516);
#4113=AXIS2_PLACEMENT_3D('',#5608,#4517,#4518);
#4114=AXIS2_PLACEMENT_3D('',#5617,#4523,#4524);
#4115=AXIS2_PLACEMENT_3D('',#5623,#4528,#4529);
#4116=AXIS2_PLACEMENT_3D('',#5632,#4534,#4535);
#4117=AXIS2_PLACEMENT_3D('',#5641,#4540,#4541);
#4118=AXIS2_PLACEMENT_3D('',#5652,#4548,#4549);
#4119=AXIS2_PLACEMENT_3D('',#5658,#4553,#4554);
#4120=AXIS2_PLACEMENT_3D('',#5669,#4561,#4562);
#4121=AXIS2_PLACEMENT_3D('',#5672,#4565,#4566);
#4122=AXIS2_PLACEMENT_3D('',#5683,#4572,#4573);
#4123=AXIS2_PLACEMENT_3D('',#5685,#4574,#4575);
#4124=AXIS2_PLACEMENT_3D('',#5686,#4576,#4577);
#4125=AXIS2_PLACEMENT_3D('',#5690,#4580,#4581);
#4126=AXIS2_PLACEMENT_3D('',#5696,#4584,#4585);
#4127=AXIS2_PLACEMENT_3D('',#5704,#4589,#4590);
#4128=AXIS2_PLACEMENT_3D('',#5708,#4593,#4594);
#4129=AXIS2_PLACEMENT_3D('',#5712,#4596,#4597);
#4130=AXIS2_PLACEMENT_3D('',#5714,#4598,#4599);
#4131=AXIS2_PLACEMENT_3D('',#5718,#4601,#4602);
#4132=AXIS2_PLACEMENT_3D('',#5719,#4603,#4604);
#4133=AXIS2_PLACEMENT_3D('',#5721,#4605,#4606);
#4134=AXIS2_PLACEMENT_3D('',#5723,#4607,#4608);
#4135=AXIS2_PLACEMENT_3D('',#5746,#4609,#4610);
#4136=AXIS2_PLACEMENT_3D('',#5752,#4611,#4612);
#4137=AXIS2_PLACEMENT_3D('',#5757,#4613,#4614);
#4138=AXIS2_PLACEMENT_3D('',#5760,#4615,#4616);
#4139=AXIS2_PLACEMENT_3D('',#5761,#4617,#4618);
#4140=AXIS2_PLACEMENT_3D('',#5762,#4619,#4620);
#4141=AXIS2_PLACEMENT_3D('',#5789,#4621,#4622);
#4142=AXIS2_PLACEMENT_3D('',#5830,#4623,#4624);
#4143=AXIS2_PLACEMENT_3D('',#5831,#4625,#4626);
#4144=AXIS2_PLACEMENT_3D('',#5832,#4627,#4628);
#4145=AXIS2_PLACEMENT_3D('',#5850,#4629,#4630);
#4146=AXIS2_PLACEMENT_3D('',#5851,#4631,#4632);
#4147=AXIS2_PLACEMENT_3D('',#5852,#4633,#4634);
#4148=AXIS2_PLACEMENT_3D('',#5853,#4635,#4636);
#4149=AXIS2_PLACEMENT_3D('',#5855,#4637,#4638);
#4150=AXIS2_PLACEMENT_3D('',#5857,#4640,#4641);
#4151=AXIS2_PLACEMENT_3D('',#5858,#4642,#4643);
#4152=AXIS2_PLACEMENT_3D('',#5859,#4644,#4645);
#4153=AXIS2_PLACEMENT_3D('',#5863,#4647,#4648);
#4154=AXIS2_PLACEMENT_3D('',#5865,#4650,#4651);
#4155=AXIS2_PLACEMENT_3D('',#5868,#4653,#4654);
#4156=AXIS2_PLACEMENT_3D('',#5869,#4655,#4656);
#4157=AXIS2_PLACEMENT_3D('',#5871,#4658,#4659);
#4158=AXIS2_PLACEMENT_3D('',#5884,#4667,#4668);
#4159=AXIS2_PLACEMENT_3D('',#5901,#4669,#4670);
#4160=AXIS2_PLACEMENT_3D('',#5903,#4671,#4672);
#4161=AXIS2_PLACEMENT_3D('',#5904,#4673,#4674);
#4162=AXIS2_PLACEMENT_3D('',#5905,#4675,#4676);
#4163=AXIS2_PLACEMENT_3D('',#5907,#4677,#4678);
#4164=AXIS2_PLACEMENT_3D('',#5931,#4680,#4681);
#4165=AXIS2_PLACEMENT_3D('',#5937,#4682,#4683);
#4166=AXIS2_PLACEMENT_3D('',#5942,#4684,#4685);
#4167=AXIS2_PLACEMENT_3D('',#5945,#4686,#4687);
#4168=AXIS2_PLACEMENT_3D('',#5946,#4688,#4689);
#4169=AXIS2_PLACEMENT_3D('',#5947,#4690,#4691);
#4170=AXIS2_PLACEMENT_3D('',#5970,#4692,#4693);
#4171=AXIS2_PLACEMENT_3D('',#6010,#4694,#4695);
#4172=AXIS2_PLACEMENT_3D('',#6011,#4696,#4697);
#4173=AXIS2_PLACEMENT_3D('',#6012,#4698,#4699);
#4174=AXIS2_PLACEMENT_3D('',#6013,#4700,#4701);
#4175=AXIS2_PLACEMENT_3D('',#6014,#4702,#4703);
#4176=AXIS2_PLACEMENT_3D('',#6017,#4705,#4706);
#4177=AXIS2_PLACEMENT_3D('',#6018,#4707,#4708);
#4178=AXIS2_PLACEMENT_3D('',#6021,#4711,#4712);
#4179=AXIS2_PLACEMENT_3D('',#6054,#4713,#4714);
#4180=AXIS2_PLACEMENT_3D('',#6055,#4715,#4716);
#4181=AXIS2_PLACEMENT_3D('',#6056,#4717,#4718);
#4182=AXIS2_PLACEMENT_3D('',#6083,#4719,#4720);
#4183=AXIS2_PLACEMENT_3D('',#6088,#4721,#4722);
#4184=AXIS2_PLACEMENT_3D('',#6091,#4723,#4724);
#4185=AXIS2_PLACEMENT_3D('',#6092,#4725,#4726);
#4186=AXIS2_PLACEMENT_3D('',#6093,#4727,#4728);
#4187=AXIS2_PLACEMENT_3D('',#6150,#4729,#4730);
#4188=AXIS2_PLACEMENT_3D('',#6154,#4732,#4733);
#4189=AXIS2_PLACEMENT_3D('',#6156,#4735,#4736);
#4190=AXIS2_PLACEMENT_3D('',#6167,#4739,#4740);
#4191=AXIS2_PLACEMENT_3D('',#6199,#4741,#4742);
#4192=AXIS2_PLACEMENT_3D('',#6201,#4743,#4744);
#4193=AXIS2_PLACEMENT_3D('',#6202,#4745,#4746);
#4194=AXIS2_PLACEMENT_3D('',#6203,#4747,#4748);
#4195=AXIS2_PLACEMENT_3D('',#6206,#4749,#4750);
#4196=AXIS2_PLACEMENT_3D('',#6208,#4751,#4752);
#4197=AXIS2_PLACEMENT_3D('',#6210,#4753,#4754);
#4198=AXIS2_PLACEMENT_3D('',#6211,#4755,#4756);
#4199=AXIS2_PLACEMENT_3D('',#6238,#4757,#4758);
#4200=AXIS2_PLACEMENT_3D('',#6279,#4759,#4760);
#4201=AXIS2_PLACEMENT_3D('',#6280,#4761,#4762);
#4202=AXIS2_PLACEMENT_3D('',#6338,#4763,#4764);
#4203=AXIS2_PLACEMENT_3D('',#6341,#4767,#4768);
#4204=AXIS2_PLACEMENT_3D('',#6344,#4770,#4771);
#4205=AXIS2_PLACEMENT_3D('',#6346,#4773,#4774);
#4206=AXIS2_PLACEMENT_3D('',#6355,#4776,#4777);
#4207=AXIS2_PLACEMENT_3D('',#6357,#4778,#4779);
#4208=AXIS2_PLACEMENT_3D('',#6391,#4780,#4781);
#4209=AXIS2_PLACEMENT_3D('',#6392,#4782,#4783);
#4210=AXIS2_PLACEMENT_3D('',#6393,#4784,#4785);
#4211=AXIS2_PLACEMENT_3D('',#6397,#4787,#4788);
#4212=AXIS2_PLACEMENT_3D('',#6399,#4790,#4791);
#4213=AXIS2_PLACEMENT_3D('',#6402,#4792,#4793);
#4214=AXIS2_PLACEMENT_3D('',#6404,#4794,#4795);
#4215=AXIS2_PLACEMENT_3D('',#6406,#4796,#4797);
#4216=AXIS2_PLACEMENT_3D('',#6419,#4798,#4799);
#4217=AXIS2_PLACEMENT_3D('',#6422,#4800,#4801);
#4218=AXIS2_PLACEMENT_3D('',#6446,#4804,#4805);
#4219=AXIS2_PLACEMENT_3D('',#6448,#4806,#4807);
#4220=AXIS2_PLACEMENT_3D('',#6450,#4808,#4809);
#4221=AXIS2_PLACEMENT_3D('',#6510,#4810,#4811);
#4222=AXIS2_PLACEMENT_3D('',#6511,#4812,#4813);
#4223=AXIS2_PLACEMENT_3D('',#6512,#4814,#4815);
#4224=AXIS2_PLACEMENT_3D('',#6534,#4816,#4817);
#4225=AXIS2_PLACEMENT_3D('',#6536,#4818,#4819);
#4226=AXIS2_PLACEMENT_3D('',#6600,#4820,#4821);
#4227=AXIS2_PLACEMENT_3D('',#6602,#4822,#4823);
#4228=AXIS2_PLACEMENT_3D('',#6604,#4824,#4825);
#4229=AXIS2_PLACEMENT_3D('',#6605,#4826,#4827);
#4230=AXIS2_PLACEMENT_3D('',#6606,#4828,#4829);
#4231=AXIS2_PLACEMENT_3D('',#6608,#4830,#4831);
#4232=AXIS2_PLACEMENT_3D('',#6611,#4834,#4835);
#4233=AXIS2_PLACEMENT_3D('',#6612,#4836,#4837);
#4234=AXIS2_PLACEMENT_3D('',#6614,#4839,#4840);
#4235=AXIS2_PLACEMENT_3D('',#6615,#4841,#4842);
#4236=AXIS2_PLACEMENT_3D('',#6616,#4843,#4844);
#4237=AXIS2_PLACEMENT_3D('',#6617,#4845,#4846);
#4238=AXIS2_PLACEMENT_3D('',#6618,#4847,#4848);
#4239=AXIS2_PLACEMENT_3D('',#6620,#4850,#4851);
#4240=AXIS2_PLACEMENT_3D('',#6628,#4857,#4858);
#4241=AXIS2_PLACEMENT_3D('',#6631,#4860,#4861);
#4242=AXIS2_PLACEMENT_3D('',#6632,#4862,#4863);
#4243=AXIS2_PLACEMENT_3D('',#6636,#4866,#4867);
#4244=AXIS2_PLACEMENT_3D('',#6639,#4869,#4870);
#4245=AXIS2_PLACEMENT_3D('',#6640,#4871,#4872);
#4246=AXIS2_PLACEMENT_3D('',#6643,#4874,#4875);
#4247=AXIS2_PLACEMENT_3D('',#6644,#4876,#4877);
#4248=AXIS2_PLACEMENT_3D('',#6647,#4879,#4880);
#4249=AXIS2_PLACEMENT_3D('',#6648,#4881,#4882);
#4250=AXIS2_PLACEMENT_3D('',#6652,#4885,#4886);
#4251=AXIS2_PLACEMENT_3D('',#6653,#4887,#4888);
#4252=AXIS2_PLACEMENT_3D('',#6654,#4889,#4890);
#4253=AXIS2_PLACEMENT_3D('',#6657,#4892,#4893);
#4254=AXIS2_PLACEMENT_3D('',#6658,#4894,#4895);
#4255=AXIS2_PLACEMENT_3D('',#6661,#4896,#4897);
#4256=AXIS2_PLACEMENT_3D('',#6662,#4898,#4899);
#4257=AXIS2_PLACEMENT_3D('',#6664,#4901,#4902);
#4258=AXIS2_PLACEMENT_3D('',#6667,#4905,#4906);
#4259=AXIS2_PLACEMENT_3D('',#6668,#4907,#4908);
#4260=AXIS2_PLACEMENT_3D('',#6669,#4909,#4910);
#4261=AXIS2_PLACEMENT_3D('',#6671,#4912,#4913);
#4262=AXIS2_PLACEMENT_3D('',#6673,#4914,#4915);
#4263=AXIS2_PLACEMENT_3D('',#6674,#4916,#4917);
#4264=AXIS2_PLACEMENT_3D('',#6675,#4918,#4919);
#4265=AXIS2_PLACEMENT_3D('',#6678,#4921,#4922);
#4266=AXIS2_PLACEMENT_3D('',#6679,#4923,#4924);
#4267=AXIS2_PLACEMENT_3D('',#6680,#4925,#4926);
#4268=AXIS2_PLACEMENT_3D('',#6681,#4927,#4928);
#4269=AXIS2_PLACEMENT_3D('',#6683,#4930,#4931);
#4270=AXIS2_PLACEMENT_3D('',#6686,#4933,#4934);
#4271=AXIS2_PLACEMENT_3D('',#6687,#4935,#4936);
#4272=AXIS2_PLACEMENT_3D('',#6689,#4938,#4939);
#4273=AXIS2_PLACEMENT_3D('',#6691,#4941,#4942);
#4274=AXIS2_PLACEMENT_3D('',#6693,#4943,#4944);
#4275=AXIS2_PLACEMENT_3D('',#6696,#4946,#4947);
#4276=AXIS2_PLACEMENT_3D('',#6698,#4949,#4950);
#4277=AXIS2_PLACEMENT_3D('',#6700,#4951,#4952);
#4278=AXIS2_PLACEMENT_3D('',#6703,#4954,#4955);
#4279=AXIS2_PLACEMENT_3D('',#6705,#4957,#4958);
#4280=AXIS2_PLACEMENT_3D('',#6706,#4959,#4960);
#4281=AXIS2_PLACEMENT_3D('',#6708,#4962,#4963);
#4282=AXIS2_PLACEMENT_3D('',#6709,#4964,#4965);
#4283=AXIS2_PLACEMENT_3D('',#6711,#4967,#4968);
#4284=AXIS2_PLACEMENT_3D('',#6712,#4969,#4970);
#4285=AXIS2_PLACEMENT_3D('',#6713,#4971,#4972);
#4286=AXIS2_PLACEMENT_3D('',#6715,#4973,#4974);
#4287=AXIS2_PLACEMENT_3D('',#6718,#4976,#4977);
#4288=AXIS2_PLACEMENT_3D('',#6719,#4978,#4979);
#4289=AXIS2_PLACEMENT_3D('',#6720,#4980,#4981);
#4290=AXIS2_PLACEMENT_3D('',#6722,#4982,#4983);
#4291=AXIS2_PLACEMENT_3D('',#6725,#4985,#4986);
#4292=AXIS2_PLACEMENT_3D('',#6726,#4987,#4988);
#4293=AXIS2_PLACEMENT_3D('',#7349,#4990,#4991);
#4294=AXIS2_PLACEMENT_3D('',#7353,#4994,#4995);
#4295=AXIS2_PLACEMENT_3D('',#7357,#4997,#4998);
#4296=AXIS2_PLACEMENT_3D('',#7360,#5000,#5001);
#4297=AXIS2_PLACEMENT_3D('',#7361,#5002,#5003);
#4298=AXIS2_PLACEMENT_3D('',#7879,#5005,#5006);
#4299=AXIS2_PLACEMENT_3D('',#7883,#5008,#5009);
#4300=AXIS2_PLACEMENT_3D('',#7886,#5012,#5013);
#4301=AXIS2_PLACEMENT_3D('',#7888,#5015,#5016);
#4302=AXIS2_PLACEMENT_3D('',#7890,#5018,#5019);
#4303=AXIS2_PLACEMENT_3D('',#7892,#5021,#5022);
#4304=AXIS2_PLACEMENT_3D('',#7894,#5024,#5025);
#4305=AXIS2_PLACEMENT_3D('',#7896,#5027,#5028);
#4306=AXIS2_PLACEMENT_3D('',#7898,#5030,#5031);
#4307=AXIS2_PLACEMENT_3D('',#7902,#5033,#5034);
#4308=AXIS2_PLACEMENT_3D('',#7904,#5036,#5037);
#4309=AXIS2_PLACEMENT_3D('',#7908,#5039,#5040);
#4310=AXIS2_PLACEMENT_3D('',#7910,#5042,#5043);
#4311=AXIS2_PLACEMENT_3D('',#7916,#5047,#5048);
#4312=AXIS2_PLACEMENT_3D('',#7920,#5051,#5052);
#4313=AXIS2_PLACEMENT_3D('',#7924,#5055,#5056);
#4314=AXIS2_PLACEMENT_3D('',#7926,#5058,#5059);
#4315=AXIS2_PLACEMENT_3D('',#7928,#5061,#5062);
#4316=AXIS2_PLACEMENT_3D('',#7930,#5063,#5064);
#4317=AXIS2_PLACEMENT_3D('',#7934,#5066,#5067);
#4318=AXIS2_PLACEMENT_3D('',#7936,#5069,#5070);
#4319=AXIS2_PLACEMENT_3D('',#7942,#5074,#5075);
#4320=AXIS2_PLACEMENT_3D('',#7944,#5076,#5077);
#4321=AXIS2_PLACEMENT_3D('',#7947,#5079,#5080);
#4322=AXIS2_PLACEMENT_3D('',#7948,#5081,#5082);
#4323=AXIS2_PLACEMENT_3D('',#7962,#5090,#5091);
#4324=AXIS2_PLACEMENT_3D('',#7966,#5094,#5095);
#4325=AXIS2_PLACEMENT_3D('',#7970,#5098,#5099);
#4326=AXIS2_PLACEMENT_3D('',#7974,#5102,#5103);
#4327=AXIS2_PLACEMENT_3D('',#7978,#5106,#5107);
#4328=AXIS2_PLACEMENT_3D('',#7980,#5108,#5109);
#4329=AXIS2_PLACEMENT_3D('',#7983,#5111,#5112);
#4330=AXIS2_PLACEMENT_3D('',#7985,#5113,#5114);
#4331=AXIS2_PLACEMENT_3D('',#7987,#5116,#5117);
#4332=AXIS2_PLACEMENT_3D('',#7989,#5118,#5119);
#4333=AXIS2_PLACEMENT_3D('',#7992,#5121,#5122);
#4334=AXIS2_PLACEMENT_3D('',#7993,#5123,#5124);
#4335=AXIS2_PLACEMENT_3D('',#7994,#5125,#5126);
#4336=AXIS2_PLACEMENT_3D('',#8003,#5131,#5132);
#4337=AXIS2_PLACEMENT_3D('',#8009,#5136,#5137);
#4338=AXIS2_PLACEMENT_3D('',#8018,#5143,#5144);
#4339=AXIS2_PLACEMENT_3D('',#8022,#5147,#5148);
#4340=AXIS2_PLACEMENT_3D('',#8026,#5151,#5152);
#4341=AXIS2_PLACEMENT_3D('',#8028,#5154,#5155);
#4342=AXIS2_PLACEMENT_3D('',#8031,#5158,#5159);
#4343=AXIS2_PLACEMENT_3D('',#8032,#5160,#5161);
#4344=AXIS2_PLACEMENT_3D('',#8033,#5162,#5163);
#4345=AXIS2_PLACEMENT_3D('',#8034,#5164,#5165);
#4346=AXIS2_PLACEMENT_3D('',#8036,#5166,#5167);
#4347=AXIS2_PLACEMENT_3D('',#8038,#5168,#5169);
#4348=AXIS2_PLACEMENT_3D('',#8039,#5170,#5171);
#4349=AXIS2_PLACEMENT_3D('',#8041,#5172,#5173);
#4350=AXIS2_PLACEMENT_3D('',#8043,#5175,#5176);
#4351=AXIS2_PLACEMENT_3D('',#8046,#5178,#5179);
#4352=AXIS2_PLACEMENT_3D('',#8047,#5180,#5181);
#4353=AXIS2_PLACEMENT_3D('',#8049,#5182,#5183);
#4354=AXIS2_PLACEMENT_3D('',#8051,#5184,#5185);
#4355=AXIS2_PLACEMENT_3D('',#8052,#5186,#5187);
#4356=AXIS2_PLACEMENT_3D('',#8054,#5188,#5189);
#4357=AXIS2_PLACEMENT_3D('',#8056,#5191,#5192);
#4358=AXIS2_PLACEMENT_3D('',#8059,#5194,#5195);
#4359=AXIS2_PLACEMENT_3D('',#8060,#5196,#5197);
#4360=AXIS2_PLACEMENT_3D('',#8069,#5202,#5203);
#4361=AXIS2_PLACEMENT_3D('',#8075,#5207,#5208);
#4362=AXIS2_PLACEMENT_3D('',#8079,#5211,#5212);
#4363=AXIS2_PLACEMENT_3D('',#8083,#5215,#5216);
#4364=AXIS2_PLACEMENT_3D('',#8085,#5218,#5219);
#4365=AXIS2_PLACEMENT_3D('',#8086,#5220,#5221);
#4366=AXIS2_PLACEMENT_3D('',#8087,#5222,#5223);
#4367=AXIS2_PLACEMENT_3D('',#8090,#5224,#5225);
#4368=AXIS2_PLACEMENT_3D('',#8092,#5226,#5227);
#4369=AXIS2_PLACEMENT_3D('',#8093,#5228,#5229);
#4370=AXIS2_PLACEMENT_3D('',#8094,#5230,#5231);
#4371=AXIS2_PLACEMENT_3D('',#8095,#5232,#5233);
#4372=AXIS2_PLACEMENT_3D('',#8097,#5234,#5235);
#4373=AXIS2_PLACEMENT_3D('',#8099,#5237,#5238);
#4374=AXIS2_PLACEMENT_3D('',#8101,#5239,#5240);
#4375=AXIS2_PLACEMENT_3D('',#8102,#5241,#5242);
#4376=AXIS2_PLACEMENT_3D('',#8111,#5247,#5248);
#4377=AXIS2_PLACEMENT_3D('',#8117,#5252,#5253);
#4378=AXIS2_PLACEMENT_3D('',#8123,#5257,#5258);
#4379=AXIS2_PLACEMENT_3D('',#8129,#5262,#5263);
#4380=AXIS2_PLACEMENT_3D('',#8135,#5267,#5268);
#4381=AXIS2_PLACEMENT_3D('',#8138,#5271,#5272);
#4382=AXIS2_PLACEMENT_3D('',#8139,#5273,#5274);
#4383=AXIS2_PLACEMENT_3D('',#8141,#5275,#5276);
#4384=AXIS2_PLACEMENT_3D('',#8143,#5277,#5278);
#4385=AXIS2_PLACEMENT_3D('',#8145,#5279,#5280);
#4386=AXIS2_PLACEMENT_3D('',#8146,#5281,#5282);
#4387=AXIS2_PLACEMENT_3D('',#8147,#5283,#5284);
#4388=AXIS2_PLACEMENT_3D('',#8149,#5286,#5287);
#4389=AXIS2_PLACEMENT_3D('',#8150,#5288,#5289);
#4390=AXIS2_PLACEMENT_3D('',#8151,#5290,#5291);
#4391=AXIS2_PLACEMENT_3D('',#8152,#5292,#5293);
#4392=AXIS2_PLACEMENT_3D('',#8155,#5294,#5295);
#4393=AXIS2_PLACEMENT_3D('',#8159,#5297,#5298);
#4394=AXIS2_PLACEMENT_3D('',#8161,#5300,#5301);
#4395=AXIS2_PLACEMENT_3D('',#8167,#5305,#5306);
#4396=AXIS2_PLACEMENT_3D('',#8176,#5311,#5312);
#4397=AXIS2_PLACEMENT_3D('',#8182,#5316,#5317);
#4398=AXIS2_PLACEMENT_3D('',#8191,#5322,#5323);
#4399=AXIS2_PLACEMENT_3D('',#8192,#5324,#5325);
#4400=AXIS2_PLACEMENT_3D('',#8193,#5326,#5327);
#4401=AXIS2_PLACEMENT_3D('',#8194,#5328,#5329);
#4402=AXIS2_PLACEMENT_3D('',#8196,#5330,#5331);
#4403=AXIS2_PLACEMENT_3D('',#8197,#5332,#5333);
#4404=AXIS2_PLACEMENT_3D('',#8199,#5334,#5335);
#4405=AXIS2_PLACEMENT_3D('',#8200,#5336,#5337);
#4406=AXIS2_PLACEMENT_3D('',#8201,#5338,#5339);
#4407=AXIS2_PLACEMENT_3D('',#8202,#5340,#5341);
#4408=AXIS2_PLACEMENT_3D('',#8203,#5342,#5343);
#4409=AXIS2_PLACEMENT_3D('',#8204,#5344,#5345);
#4410=AXIS2_PLACEMENT_3D('',#8207,#5347,#5348);
#4411=AXIS2_PLACEMENT_3D('',#8208,#5349,#5350);
#4412=AXIS2_PLACEMENT_3D('',#8211,#5352,#5353);
#4413=AXIS2_PLACEMENT_3D('',#8212,#5354,#5355);
#4414=AXIS2_PLACEMENT_3D('',#8213,#5356,#5357);
#4415=AXIS2_PLACEMENT_3D('',#8214,#5358,#5359);
#4416=AXIS2_PLACEMENT_3D('',#8216,#5360,#5361);
#4417=AXIS2_PLACEMENT_3D('',#8219,#5363,#5364);
#4418=AXIS2_PLACEMENT_3D('',#8220,#5365,#5366);
#4419=AXIS2_PLACEMENT_3D('',#8223,#5367,#5368);
#4420=AXIS2_PLACEMENT_3D('',#8227,#5370,#5371);
#4421=AXIS2_PLACEMENT_3D('',#8229,#5373,#5374);
#4422=AXIS2_PLACEMENT_3D('',#8235,#5378,#5379);
#4423=AXIS2_PLACEMENT_3D('',#8237,#5380,#5381);
#4424=AXIS2_PLACEMENT_3D('',#8239,#5382,#5383);
#4425=AXIS2_PLACEMENT_3D('',#8241,#5385,#5386);
#4426=AXIS2_PLACEMENT_3D('',#8243,#5387,#5388);
#4427=AXIS2_PLACEMENT_3D('',#8245,#5389,#5390);
#4428=AXIS2_PLACEMENT_3D('',#8247,#5392,#5393);
#4429=AXIS2_PLACEMENT_3D('',#8249,#5394,#5395);
#4430=AXIS2_PLACEMENT_3D('',#8251,#5396,#5397);
#4431=AXIS2_PLACEMENT_3D('',#8253,#5399,#5400);
#4432=AXIS2_PLACEMENT_3D('',#8256,#5403,#5404);
#4433=AXIS2_PLACEMENT_3D('',#8257,#5405,#5406);
#4434=AXIS2_PLACEMENT_3D('',#8258,#5407,#5408);
#4435=AXIS2_PLACEMENT_3D('',#8259,#5409,#5410);
#4436=AXIS2_PLACEMENT_3D('',#8268,#5415,#5416);
#4437=AXIS2_PLACEMENT_3D('',#8277,#5421,#5422);
#4438=AXIS2_PLACEMENT_3D('',#8278,#5423,#5424);
#4439=AXIS2_PLACEMENT_3D('',#8279,#5425,#5426);
#4440=AXIS2_PLACEMENT_3D('',#8280,#5427,#5428);
#4441=AXIS2_PLACEMENT_3D('',#8282,#5429,#5430);
#4442=AXIS2_PLACEMENT_3D('',#8283,#5431,#5432);
#4443=AXIS2_PLACEMENT_3D('',#8284,#5433,#5434);
#4444=AXIS2_PLACEMENT_3D('',#8285,#5435,#5436);
#4445=AXIS2_PLACEMENT_3D('',#8286,#5437,#5438);
#4446=AXIS2_PLACEMENT_3D('',#8288,#5439,#5440);
#4447=AXIS2_PLACEMENT_3D('',#8291,#5442,#5443);
#4448=AXIS2_PLACEMENT_3D('',#8292,#5444,#5445);
#4449=AXIS2_PLACEMENT_3D('',#8293,#5446,#5447);
#4450=AXIS2_PLACEMENT_3D('',#8295,#5448,#5449);
#4451=AXIS2_PLACEMENT_3D('',#8297,#5451,#5452);
#4452=AXIS2_PLACEMENT_3D('',#8298,#5453,#5454);
#4453=AXIS2_PLACEMENT_3D('',#8299,#5455,#5456);
#4454=AXIS2_PLACEMENT_3D('',#8301,#5457,#5458);
#4455=AXIS2_PLACEMENT_3D('',#8303,#5459,#5460);
#4456=AXIS2_PLACEMENT_3D('',#8305,#5461,#5462);
#4457=AXIS2_PLACEMENT_3D('',#8306,#5463,#5464);
#4458=AXIS2_PLACEMENT_3D('',#8307,#5465,#5466);
#4459=AXIS2_PLACEMENT_3D('',#8311,#5468,#5469);
#4460=AXIS2_PLACEMENT_3D('',#8312,#5470,#5471);
#4461=AXIS2_PLACEMENT_3D('',#8313,#5472,#5473);
#4462=AXIS2_PLACEMENT_3D('',#8314,#5474,#5475);
#4463=AXIS2_PLACEMENT_3D('',#8317,#5476,#5477);
#4464=AXIS2_PLACEMENT_3D('',#8318,#5478,#5479);
#4465=AXIS2_PLACEMENT_3D('',#8319,#5480,#5481);
#4466=AXIS2_PLACEMENT_3D('',#8320,#5482,#5483);
#4467=AXIS2_PLACEMENT_3D('',#8323,#5485,#5486);
#4468=AXIS2_PLACEMENT_3D('',#8324,#5487,#5488);
#4469=AXIS2_PLACEMENT_3D('',#8326,#5489,#5490);
#4470=AXIS2_PLACEMENT_3D('',#8327,#5491,#5492);
#4471=AXIS2_PLACEMENT_3D('',#8330,#5494,#5495);
#4472=AXIS2_PLACEMENT_3D('',#8331,#5496,#5497);
#4473=AXIS2_PLACEMENT_3D('',#8333,#5498,#5499);
#4474=AXIS2_PLACEMENT_3D('',#8335,#5500,#5501);
#4475=AXIS2_PLACEMENT_3D('',#8336,#5502,#5503);
#4476=AXIS2_PLACEMENT_3D('',#8338,#5504,#5505);
#4477=AXIS2_PLACEMENT_3D('',#8340,#5507,#5508);
#4478=AXIS2_PLACEMENT_3D('',#8341,#5509,#5510);
#4479=AXIS2_PLACEMENT_3D('',#8344,#5512,#5513);
#4480=AXIS2_PLACEMENT_3D('',#8345,#5514,#5515);
#4481=AXIS2_PLACEMENT_3D('',#8347,#5516,#5517);
#4482=AXIS2_PLACEMENT_3D('',#8350,#5519,#5520);
#4483=AXIS2_PLACEMENT_3D('',#8351,#5521,#5522);
#4484=AXIS2_PLACEMENT_3D('',#8352,#5523,#5524);
#4485=AXIS2_PLACEMENT_3D('',#8354,#5525,#5526);
#4486=AXIS2_PLACEMENT_3D('',#8357,#5528,#5529);
#4487=AXIS2_PLACEMENT_3D('',#8358,#5530,#5531);
#4488=AXIS2_PLACEMENT_3D('',#8359,#5532,#5533);
#4489=AXIS2_PLACEMENT_3D('',#8360,#5534,#5535);
#4490=AXIS2_PLACEMENT_3D('',#8361,#5536,#5537);
#4491=AXIS2_PLACEMENT_3D('',#8370,#5542,#5543);
#4492=AXIS2_PLACEMENT_3D('',#8376,#5547,#5548);
#4493=AXIS2_PLACEMENT_3D('',#8382,#5552,#5553);
#4494=AXIS2_PLACEMENT_3D('',#8388,#5557,#5558);
#4495=AXIS2_PLACEMENT_3D('',#8394,#5562,#5563);
#4496=AXIS2_PLACEMENT_3D('',#8400,#5567,#5568);
#4497=AXIS2_PLACEMENT_3D('',#8406,#5572,#5573);
#4498=AXIS2_PLACEMENT_3D('',#8409,#5576,#5577);
#4499=AXIS2_PLACEMENT_3D('',#8410,#5578,#5579);
#4500=AXIS2_PLACEMENT_3D('',#8411,#5580,#5581);
#4501=AXIS2_PLACEMENT_3D('',#8412,#5582,#5583);
#4502=AXIS2_PLACEMENT_3D('',#8413,#5584,#5585);
#4503=AXIS2_PLACEMENT_3D('',#8414,#5586,#5587);
#4504=AXIS2_PLACEMENT_3D('',#8415,#5588,#5589);
#4505=AXIS2_PLACEMENT_3D('',#8416,#5590,#5591);
#4506=AXIS2_PLACEMENT_3D('',#8417,#5592,#5593);
#4507=AXIS2_PLACEMENT_3D('',#8418,#5594,#5595);
#4508=AXIS2_PLACEMENT_3D('',#8419,#5596,#5597);
#4509=AXIS2_PLACEMENT_3D('',#8420,#5598,#5599);
#4510=AXIS2_PLACEMENT_3D('',#8421,#5600,#5601);
#4511=AXIS2_PLACEMENT_3D('',#8422,#5602,#5603);
#4512=AXIS2_PLACEMENT_3D('',#8423,#5604,#5605);
#4513=DIRECTION('axis',(0.,0.,1.));
#4514=DIRECTION('refdir',(1.,0.,0.));
#4515=DIRECTION('axis',(0.,0.,1.));
#4516=DIRECTION('refdir',(1.,0.,0.));
#4517=DIRECTION('center_axis',(-0.00925888381263175,0.,0.999957135616594));
#4518=DIRECTION('ref_axis',(0.,1.,0.));
#4519=DIRECTION('',(0.,-1.,0.));
#4520=DIRECTION('',(-0.999957135616594,0.,-0.00925888381263175));
#4521=DIRECTION('',(0.,1.,0.));
#4522=DIRECTION('',(-0.999957135616594,0.,-0.00925888381263175));
#4523=DIRECTION('center_axis',(0.,-1.,0.));
#4524=DIRECTION('ref_axis',(-0.00925888381263175,0.,0.999957135616594));
#4525=DIRECTION('',(0.,0.,-1.));
#4526=DIRECTION('',(-0.00925888381263175,0.,0.999957135616594));
#4527=DIRECTION('',(1.,0.,0.));
#4528=DIRECTION('center_axis',(0.,1.,0.));
#4529=DIRECTION('ref_axis',(0.00925888381263175,0.,-0.999957135616594));
#4530=DIRECTION('',(-1.,0.,0.));
#4531=DIRECTION('',(0.00925888381263175,0.,-0.999957135616594));
#4532=DIRECTION('',(-0.999957135616594,0.,-0.00925888381263175));
#4533=DIRECTION('',(0.,0.,1.));
#4534=DIRECTION('center_axis',(-0.00925888381263175,0.,0.999957135616594));
#4535=DIRECTION('ref_axis',(0.,1.,0.));
#4536=DIRECTION('',(0.,-1.,0.));
#4537=DIRECTION('',(-0.999957135616594,0.,-0.00925888381263175));
#4538=DIRECTION('',(0.,1.,0.));
#4539=DIRECTION('',(-0.999957135616594,0.,-0.00925888381263175));
#4540=DIRECTION('center_axis',(0.,-1.,0.));
#4541=DIRECTION('ref_axis',(-0.00925888381263175,0.,0.999957135616594));
#4542=DIRECTION('',(0.,0.,-1.));
#4543=DIRECTION('',(-0.999957135616594,0.,-0.00925888381263175));
#4544=DIRECTION('',(0.,0.,1.));
#4545=DIRECTION('',(-1.,0.,0.));
#4546=DIRECTION('',(0.,0.,-1.));
#4547=DIRECTION('',(-0.00925888381263175,0.,0.999957135616594));
#4548=DIRECTION('center_axis',(-0.00925888381263175,0.,0.999957135616594));
#4549=DIRECTION('ref_axis',(0.,1.,0.));
#4550=DIRECTION('',(0.,-1.,0.));
#4551=DIRECTION('',(0.,1.,0.));
#4552=DIRECTION('',(-0.999957135616594,0.,-0.00925888381263175));
#4553=DIRECTION('center_axis',(0.,1.,0.));
#4554=DIRECTION('ref_axis',(0.00925888381263175,0.,-0.999957135616594));
#4555=DIRECTION('',(0.,0.,1.));
#4556=DIRECTION('',(0.00925888381263175,0.,-0.999957135616594));
#4557=DIRECTION('',(0.,0.,1.));
#4558=DIRECTION('',(1.,0.,0.));
#4559=DIRECTION('',(0.,0.,-1.));
#4560=DIRECTION('',(-0.999957135616594,0.,-0.00925888381263175));
#4561=DIRECTION('center_axis',(-0.00925888381263175,0.,0.999957135616594));
#4562=DIRECTION('ref_axis',(0.,1.,0.));
#4563=DIRECTION('',(0.,-1.,0.));
#4564=DIRECTION('',(0.,1.,0.));
#4565=DIRECTION('center_axis',(1.,0.,0.));
#4566=DIRECTION('ref_axis',(0.,0.,-1.));
#4567=DIRECTION('',(0.,1.,0.));
#4568=DIRECTION('',(0.,0.,-1.));
#4569=DIRECTION('',(0.,1.,0.));
#4570=DIRECTION('',(0.,0.,1.));
#4571=DIRECTION('',(0.,1.,0.));
#4572=DIRECTION('center_axis',(-1.,0.,0.));
#4573=DIRECTION('ref_axis',(0.,1.,0.));
#4574=DIRECTION('center_axis',(-1.,0.,0.));
#4575=DIRECTION('ref_axis',(0.,1.,0.));
#4576=DIRECTION('center_axis',(0.,0.,1.));
#4577=DIRECTION('ref_axis',(1.,0.,0.));
#4578=DIRECTION('',(0.,1.,0.));
#4579=DIRECTION('',(1.,0.,0.));
#4580=DIRECTION('center_axis',(-1.,0.,0.));
#4581=DIRECTION('ref_axis',(0.,0.,1.));
#4582=DIRECTION('',(0.,1.,0.));
#4583=DIRECTION('',(0.,0.,-1.));
#4584=DIRECTION('center_axis',(-1.,0.,0.));
#4585=DIRECTION('ref_axis',(0.,1.,0.));
#4586=DIRECTION('',(0.,0.,-1.));
#4587=DIRECTION('',(0.,1.,0.));
#4588=DIRECTION('',(0.,0.,1.));
#4589=DIRECTION('center_axis',(-1.,0.,0.));
#4590=DIRECTION('ref_axis',(0.,-1.,0.));
#4591=DIRECTION('',(0.,0.,1.));
#4592=DIRECTION('',(0.,1.,0.));
#4593=DIRECTION('center_axis',(0.,0.,-1.));
#4594=DIRECTION('ref_axis',(-1.,0.,0.));
#4595=DIRECTION('',(0.,1.,0.));
#4596=DIRECTION('center_axis',(0.,0.,1.));
#4597=DIRECTION('ref_axis',(-1.,0.,0.));
#4598=DIRECTION('center_axis',(0.,0.,-1.));
#4599=DIRECTION('ref_axis',(0.67202150503225,0.740531631177352,0.));
#4600=DIRECTION('',(1.,0.,0.));
#4601=DIRECTION('center_axis',(0.,0.,-1.));
#4602=DIRECTION('ref_axis',(-0.67202150503225,0.740531631177352,0.));
#4603=DIRECTION('center_axis',(0.,0.,1.));
#4604=DIRECTION('ref_axis',(-1.,0.,0.));
#4605=DIRECTION('center_axis',(0.,0.,-1.));
#4606=DIRECTION('ref_axis',(1.,0.,0.));
#4607=DIRECTION('center_axis',(0.,0.,-1.));
#4608=DIRECTION('ref_axis',(1.,0.,0.));
#4609=DIRECTION('center_axis',(-0.120000000000002,-0.992773891679268,-5.92281122919324E-15));
#4610=DIRECTION('ref_axis',(-3.70074341541719E-16,-5.9211894646675E-15,
1.));
#4611=DIRECTION('center_axis',(6.53807313370374E-14,0.866025403784389,-0.500000000000086));
#4612=DIRECTION('ref_axis',(-1.,7.54951656745106E-14,0.));
#4613=DIRECTION('center_axis',(0.,0.,1.));
#4614=DIRECTION('ref_axis',(1.,0.,0.));
#4615=DIRECTION('center_axis',(-0.119999999999998,0.992773891679269,0.));
#4616=DIRECTION('ref_axis',(0.,0.,1.));
#4617=DIRECTION('center_axis',(0.,0.,1.));
#4618=DIRECTION('ref_axis',(-1.58603289232165E-16,1.,0.));
#4619=DIRECTION('center_axis',(0.,0.,-1.));
#4620=DIRECTION('ref_axis',(-1.58603289232165E-16,1.,0.));
#4621=DIRECTION('center_axis',(-0.0963241948601912,0.990678201521095,-0.0963241948601896));
#4622=DIRECTION('ref_axis',(0.,0.0967741935483864,0.995306362615581));
#4623=DIRECTION('center_axis',(-0.447213595499958,0.,0.894427190999916));
#4624=DIRECTION('ref_axis',(-0.894427190999916,0.,-0.447213595499958));
#4625=DIRECTION('center_axis',(0.894427190999916,0.,-0.447213595499957));
#4626=DIRECTION('ref_axis',(-0.447213595499957,0.,-0.894427190999916));
#4627=DIRECTION('center_axis',(0.,1.,0.));
#4628=DIRECTION('ref_axis',(0.,0.,1.));
#4629=DIRECTION('center_axis',(0.,-1.,0.));
#4630=DIRECTION('ref_axis',(-0.870367380373861,0.,0.492402907364633));
#4631=DIRECTION('center_axis',(0.,0.,1.));
#4632=DIRECTION('ref_axis',(0.,1.,0.));
#4633=DIRECTION('center_axis',(0.,1.,0.));
#4634=DIRECTION('ref_axis',(-0.870367380373861,0.,0.492402907364633));
#4635=DIRECTION('center_axis',(0.,0.,1.));
#4636=DIRECTION('ref_axis',(-0.707106781186547,0.707106781186547,0.));
#4637=DIRECTION('center_axis',(0.,0.,1.));
#4638=DIRECTION('ref_axis',(0.,1.,0.));
#4639=DIRECTION('',(0.,0.,-1.));
#4640=DIRECTION('center_axis',(-1.,0.,0.));
#4641=DIRECTION('ref_axis',(0.,0.,1.));
#4642=DIRECTION('center_axis',(1.,0.,0.));
#4643=DIRECTION('ref_axis',(0.,-1.,0.));
#4644=DIRECTION('center_axis',(0.,0.,1.));
#4645=DIRECTION('ref_axis',(-0.672021505032249,-0.740531631177353,0.));
#4646=DIRECTION('',(0.,0.,-1.));
#4647=DIRECTION('center_axis',(0.,0.,-1.));
#4648=DIRECTION('ref_axis',(-0.672021505032249,-0.740531631177353,0.));
#4649=DIRECTION('',(0.,0.,1.));
#4650=DIRECTION('center_axis',(0.,0.,1.));
#4651=DIRECTION('ref_axis',(1.,0.,0.));
#4652=DIRECTION('',(-1.,0.,0.));
#4653=DIRECTION('center_axis',(0.,0.,-1.));
#4654=DIRECTION('ref_axis',(1.,0.,0.));
#4655=DIRECTION('center_axis',(-1.,0.,0.));
#4656=DIRECTION('ref_axis',(0.,-0.707106781186547,-0.707106781186548));
#4657=DIRECTION('',(1.,0.,0.));
#4658=DIRECTION('center_axis',(0.,1.,0.));
#4659=DIRECTION('ref_axis',(1.,0.,0.));
#4660=DIRECTION('',(1.,0.,0.));
#4661=DIRECTION('',(0.,0.,1.));
#4662=DIRECTION('',(-0.999957135616594,0.,-0.0092588838126317));
#4663=DIRECTION('',(-0.00925888381263175,0.,0.999957135616594));
#4664=DIRECTION('',(1.,0.,0.));
#4665=DIRECTION('',(0.,0.,1.));
#4666=DIRECTION('',(-1.,0.,0.));
#4667=DIRECTION('center_axis',(0.,-1.,0.));
#4668=DIRECTION('ref_axis',(0.,0.,-1.));
#4669=DIRECTION('center_axis',(0.,-1.,0.));
#4670=DIRECTION('ref_axis',(-0.870367380373861,0.,0.492402907364633));
#4671=DIRECTION('center_axis',(0.,0.,1.));
#4672=DIRECTION('ref_axis',(-1.,0.,0.));
#4673=DIRECTION('center_axis',(0.,1.,0.));
#4674=DIRECTION('ref_axis',(-0.870367380373861,0.,0.492402907364633));
#4675=DIRECTION('center_axis',(0.,0.,-1.));
#4676=DIRECTION('ref_axis',(-0.707106781186547,-0.707106781186547,0.));
#4677=DIRECTION('center_axis',(0.,0.,1.));
#4678=DIRECTION('ref_axis',(-1.,0.,0.));
#4679=DIRECTION('',(0.,0.,1.));
#4680=DIRECTION('center_axis',(-0.119999999999999,0.992773891679269,-6.66133814775086E-17));
#4681=DIRECTION('ref_axis',(-0.992773891679269,-0.119999999999999,0.));
#4682=DIRECTION('center_axis',(2.30755522366023E-14,-0.866025403784422,
-0.500000000000028));
#4683=DIRECTION('ref_axis',(-9.25185853854298E-16,-0.500000000000028,0.866025403784422));
#4684=DIRECTION('center_axis',(0.,0.,1.));
#4685=DIRECTION('ref_axis',(1.,0.,0.));
#4686=DIRECTION('center_axis',(-0.12,-0.992773891679269,0.));
#4687=DIRECTION('ref_axis',(0.992773891679269,-0.12,0.));
#4688=DIRECTION('center_axis',(0.,0.,-1.));
#4689=DIRECTION('ref_axis',(1.58603289232165E-16,-1.,0.));
#4690=DIRECTION('center_axis',(0.,0.,1.));
#4691=DIRECTION('ref_axis',(1.58603289232165E-16,-1.,0.));
#4692=DIRECTION('center_axis',(-0.0963241948601912,-0.990678201521095,-0.0963241948601911));
#4693=DIRECTION('ref_axis',(0.995306362615581,-0.096774193548388,-3.70074341541719E-16));
#4694=DIRECTION('center_axis',(0.894427190999916,0.,-0.447213595499957));
#4695=DIRECTION('ref_axis',(-0.447213595499957,0.,-0.894427190999916));
#4696=DIRECTION('center_axis',(-0.447213595499958,0.,0.894427190999916));
#4697=DIRECTION('ref_axis',(-0.894427190999916,0.,-0.447213595499958));
#4698=DIRECTION('center_axis',(-1.,0.,0.));
#4699=DIRECTION('ref_axis',(0.,0.,1.));
#4700=DIRECTION('center_axis',(1.,0.,0.));
#4701=DIRECTION('ref_axis',(0.,1.,0.));
#4702=DIRECTION('center_axis',(0.,0.,1.));
#4703=DIRECTION('ref_axis',(1.,0.,0.));
#4704=DIRECTION('',(1.,0.,0.));
#4705=DIRECTION('center_axis',(0.,0.,-1.));
#4706=DIRECTION('ref_axis',(1.,0.,0.));
#4707=DIRECTION('center_axis',(0.,0.,-1.));
#4708=DIRECTION('ref_axis',(-0.67202150503225,0.740531631177352,0.));
#4709=DIRECTION('',(0.,0.,-1.));
#4710=DIRECTION('',(0.,0.,1.));
#4711=DIRECTION('center_axis',(0.,0.,1.));
#4712=DIRECTION('ref_axis',(-1.,0.,0.));
#4713=DIRECTION('center_axis',(-0.0963241948601892,-0.990678201521096,0.0963241948601895));
#4714=DIRECTION('ref_axis',(0.,0.0967741935483863,0.995306362615581));
#4715=DIRECTION('center_axis',(-0.894427190999916,0.,-0.447213595499959));
#4716=DIRECTION('ref_axis',(0.447213595499958,0.,-0.894427190999916));
#4717=DIRECTION('center_axis',(0.447213595499958,0.,0.894427190999916));
#4718=DIRECTION('ref_axis',(0.894427190999916,0.,-0.447213595499958));
#4719=DIRECTION('center_axis',(-0.119999999999994,-0.992773891679269,-4.40880173115618E-15));
#4720=DIRECTION('ref_axis',(0.,-4.44089209850062E-15,1.));
#4721=DIRECTION('center_axis',(0.,0.,1.));
#4722=DIRECTION('ref_axis',(1.,0.,0.));
#4723=DIRECTION('center_axis',(-0.12,0.992773891679269,0.));
#4724=DIRECTION('ref_axis',(0.,0.,1.));
#4725=DIRECTION('center_axis',(0.,0.,1.));
#4726=DIRECTION('ref_axis',(0.0536486895476169,0.998559872070685,0.));
#4727=DIRECTION('center_axis',(0.,0.,-1.));
#4728=DIRECTION('ref_axis',(0.0536486895476169,0.998559872070685,0.));
#4729=DIRECTION('center_axis',(0.,0.,1.));
#4730=DIRECTION('ref_axis',(1.,0.,0.));
#4731=DIRECTION('',(0.,0.,1.));
#4732=DIRECTION('center_axis',(0.,0.,1.));
#4733=DIRECTION('ref_axis',(1.,0.,0.));
#4734=DIRECTION('',(0.,0.,-1.));
#4735=DIRECTION('center_axis',(0.,-1.,0.));
#4736=DIRECTION('ref_axis',(1.,0.,0.));
#4737=DIRECTION('',(-1.,0.,0.));
#4738=DIRECTION('',(0.00925888381263175,0.,-0.999957135616594));
#4739=DIRECTION('center_axis',(0.,0.,1.));
#4740=DIRECTION('ref_axis',(1.,0.,0.));
#4741=DIRECTION('center_axis',(-0.999828575531215,0.,-0.0185153868774323));
#4742=DIRECTION('ref_axis',(0.0185153868774323,0.,-0.999828575531215));
#4743=DIRECTION('center_axis',(-0.0092588838126328,-2.96046782826604E-15,
0.999957135616594));
#4744=DIRECTION('ref_axis',(0.999957135616594,0.,0.0092588838126328));
#4745=DIRECTION('center_axis',(0.999957135616594,0.,0.00925888381263175));
#4746=DIRECTION('ref_axis',(0.00925888381263175,3.70058478533254E-16,-0.999957135616594));
#4747=DIRECTION('center_axis',(0.,0.,1.));
#4748=DIRECTION('ref_axis',(1.,0.,0.));
#4749=DIRECTION('center_axis',(0.12,-0.992773891679269,7.10542735760099E-16));
#4750=DIRECTION('ref_axis',(-5.9211894646675E-15,0.,1.));
#4751=DIRECTION('center_axis',(0.,0.,1.));
#4752=DIRECTION('ref_axis',(0.0536486895476169,-0.998559872070685,0.));
#4753=DIRECTION('center_axis',(-0.12,-0.992773891679269,0.));
#4754=DIRECTION('ref_axis',(0.992773891679269,-0.12,0.));
#4755=DIRECTION('center_axis',(0.,0.,-1.));
#4756=DIRECTION('ref_axis',(0.0536486895476169,-0.998559872070685,0.));
#4757=DIRECTION('center_axis',(0.0963241948601898,-0.990678201521096,-0.0963241948601867));
#4758=DIRECTION('ref_axis',(0.,-0.0967741935483834,0.995306362615582));
#4759=DIRECTION('center_axis',(0.447213595499958,0.,0.894427190999916));
#4760=DIRECTION('ref_axis',(0.894427190999916,0.,-0.447213595499958));
#4761=DIRECTION('center_axis',(-0.894427190999916,0.,-0.447213595499959));
#4762=DIRECTION('ref_axis',(0.447213595499959,0.,-0.894427190999916));
#4763=DIRECTION('center_axis',(0.,0.,1.));
#4764=DIRECTION('ref_axis',(0.67202150503225,0.740531631177352,0.));
#4765=DIRECTION('',(0.,0.,-1.));
#4766=DIRECTION('',(0.,0.,1.));
#4767=DIRECTION('center_axis',(1.,0.,0.));
#4768=DIRECTION('ref_axis',(0.,0.707106781186547,-0.707106781186548));
#4769=DIRECTION('',(1.,0.,0.));
#4770=DIRECTION('center_axis',(-0.999828575531215,0.,-0.0185153868774323));
#4771=DIRECTION('ref_axis',(0.0185153868774323,0.,-0.999828575531215));
#4772=DIRECTION('',(-1.,0.,0.));
#4773=DIRECTION('center_axis',(0.,0.,1.));
#4774=DIRECTION('ref_axis',(1.,0.,0.));
#4775=DIRECTION('',(-1.,0.,0.));
#4776=DIRECTION('center_axis',(0.,0.,1.));
#4777=DIRECTION('ref_axis',(1.,0.,0.));
#4778=DIRECTION('center_axis',(0.,0.,-1.));
#4779=DIRECTION('ref_axis',(1.,0.,0.));
#4780=DIRECTION('center_axis',(0.999957135616594,0.,0.00925888381263175));
#4781=DIRECTION('ref_axis',(0.00925888381263175,-3.70058478533254E-16,-0.999957135616594));
#4782=DIRECTION('center_axis',(-0.0092588838126328,2.96046782826604E-15,
0.999957135616594));
#4783=DIRECTION('ref_axis',(0.,-1.,2.96059473233375E-15));
#4784=DIRECTION('center_axis',(-0.00925888381263175,0.,0.999957135616594));
#4785=DIRECTION('ref_axis',(0.707076471490368,-0.70710678118655,0.00654701953012897));
#4786=DIRECTION('',(-0.00925888381263175,0.,0.999957135616594));
#4787=DIRECTION('center_axis',(0.0092588838126328,0.,-0.999957135616594));
#4788=DIRECTION('ref_axis',(0.999957135616594,0.,0.0092588838126328));
#4789=DIRECTION('',(0.00925888381263175,0.,-0.999957135616594));
#4790=DIRECTION('center_axis',(-0.999957135616594,0.,-0.00925888381263175));
#4791=DIRECTION('ref_axis',(-0.00925888381263226,0.,0.999957135616594));
#4792=DIRECTION('center_axis',(0.999957135616594,0.,0.00925888381263175));
#4793=DIRECTION('ref_axis',(0.00886470634978,-0.288675134594812,-0.957386068233709));
#4794=DIRECTION('center_axis',(1.37059013214855E-17,-1.,-1.48023391413303E-15));
#4795=DIRECTION('ref_axis',(0.999957135616594,0.,0.0092588838126328));
#4796=DIRECTION('center_axis',(-0.999957135616594,0.,-0.00925888381263175));
#4797=DIRECTION('ref_axis',(0.00886470634977989,-0.288675134594812,-0.957386068233709));
#4798=DIRECTION('center_axis',(0.,-1.,0.));
#4799=DIRECTION('ref_axis',(0.700529451960246,0.,0.713623491020495));
#4800=DIRECTION('center_axis',(0.,-1.,0.));
#4801=DIRECTION('ref_axis',(0.999957135616594,0.,0.00925888381263269));
#4802=DIRECTION('',(0.,-1.,0.));
#4803=DIRECTION('',(0.,1.,0.));
#4804=DIRECTION('center_axis',(-0.999989286143139,2.19273273023019E-16,
0.00462899545630677));
#4805=DIRECTION('ref_axis',(-0.00462899545630677,-4.66248702327598E-14,
-0.999989286143139));
#4806=DIRECTION('center_axis',(2.89281217569941E-15,0.212757250200078,-0.977105087739953));
#4807=DIRECTION('ref_axis',(-0.0019699752792827,0.977103191762131,0.212756837365233));
#4808=DIRECTION('center_axis',(1.,0.,0.));
#4809=DIRECTION('ref_axis',(0.,-4.69665885671789E-14,-1.));
#4810=DIRECTION('center_axis',(0.,0.212757250200078,0.977105087739953));
#4811=DIRECTION('ref_axis',(-0.0019699752792827,-0.977103191762131,0.212756837365232));
#4812=DIRECTION('center_axis',(-1.,0.,0.));
#4813=DIRECTION('ref_axis',(0.,-1.76594458083507E-13,1.));
#4814=DIRECTION('center_axis',(0.999998740412341,-2.80330577459927E-16,
0.00158719051532392));
#4815=DIRECTION('ref_axis',(-0.00158719051532392,-1.7659683092229E-13,0.999998740412341));
#4816=DIRECTION('center_axis',(1.,0.,0.));
#4817=DIRECTION('ref_axis',(0.,-1.48023391413302E-15,-1.));
#4818=DIRECTION('center_axis',(-0.999989286143139,6.85228978196936E-18,
0.00462899545630677));
#4819=DIRECTION('ref_axis',(-0.00462899545630677,-1.4801546105638E-15,-0.999989286143139));
#4820=DIRECTION('center_axis',(-0.999957135616594,0.,-0.00925888381263175));
#4821=DIRECTION('ref_axis',(-0.00925888381263226,0.,0.999957135616594));
#4822=DIRECTION('center_axis',(-0.999957135616594,0.,-0.00925888381263175));
#4823=DIRECTION('ref_axis',(0.0088647063497799,0.288675134594811,-0.957386068233709));
#4824=DIRECTION('center_axis',(1.37059013214855E-17,1.,-1.48023391413302E-15));
#4825=DIRECTION('ref_axis',(-0.00925888381264173,1.48029736616688E-15,0.999957135616594));
#4826=DIRECTION('center_axis',(0.999957135616594,0.,0.00925888381263175));
#4827=DIRECTION('ref_axis',(0.00886470634978,0.288675134594811,-0.957386068233709));
#4828=DIRECTION('center_axis',(0.,-1.,0.));
#4829=DIRECTION('ref_axis',(0.700529451960246,0.,0.713623491020495));
#4830=DIRECTION('center_axis',(0.,1.,0.));
#4831=DIRECTION('ref_axis',(-0.00925888381262989,0.,0.999957135616594));
#4832=DIRECTION('',(0.,1.,0.));
#4833=DIRECTION('',(0.,-1.,0.));
#4834=DIRECTION('center_axis',(0.00925888381263175,0.,-0.999957135616594));
#4835=DIRECTION('ref_axis',(0.707076471490368,0.70710678118655,0.00654701953012897));
#4836=DIRECTION('center_axis',(0.0092588838126328,0.,-0.999957135616594));
#4837=DIRECTION('ref_axis',(0.,1.,0.));
#4838=DIRECTION('',(0.00925888381263175,0.,-0.999957135616594));
#4839=DIRECTION('center_axis',(0.404450867664508,-0.816496580927731,0.412010714640715));
#4840=DIRECTION('ref_axis',(0.571979902364718,0.577350269189621,0.582671140487942));
#4841=DIRECTION('center_axis',(0.999957135616594,0.,0.0092588838126317));
#4842=DIRECTION('ref_axis',(-0.00654701953012685,0.707106781186547,0.70707647149037));
#4843=DIRECTION('center_axis',(-0.404450867664508,-0.816496580927731,-0.412010714640715));
#4844=DIRECTION('ref_axis',(0.571979902364718,-0.577350269189621,0.582671140487942));
#4845=DIRECTION('center_axis',(0.999957135616594,0.,0.0092588838126317));
#4846=DIRECTION('ref_axis',(-0.00654701953012685,-0.707106781186547,0.70707647149037));
#4847=DIRECTION('center_axis',(0.,0.,1.));
#4848=DIRECTION('ref_axis',(-1.,0.,0.));
#4849=DIRECTION('',(0.,0.,1.));
#4850=DIRECTION('center_axis',(0.,1.,0.));
#4851=DIRECTION('ref_axis',(1.,0.,0.));
#4852=DIRECTION('',(-1.,0.,0.));
#4853=DIRECTION('',(0.999957135616594,0.,0.0092588838126317));
#4854=DIRECTION('',(0.,0.,-1.));
#4855=DIRECTION('',(-1.,0.,0.));
#4856=DIRECTION('',(-1.,0.,0.));
#4857=DIRECTION('center_axis',(-0.999957135616594,0.,-0.0092588838126317));
#4858=DIRECTION('ref_axis',(-0.00654701953012895,-0.707106781186548,0.70707647149037));
#4859=DIRECTION('',(-0.999957135616594,0.,-0.0092588838126317));
#4860=DIRECTION('center_axis',(1.,0.,0.));
#4861=DIRECTION('ref_axis',(0.,-8.99427132075075E-13,1.));
#4862=DIRECTION('center_axis',(0.0092588838126317,0.,-0.999957135616594));
#4863=DIRECTION('ref_axis',(0.,-1.,0.));
#4864=DIRECTION('',(0.999957135616594,0.,0.00925888381263174));
#4865=DIRECTION('',(0.,1.,0.));
#4866=DIRECTION('center_axis',(-0.999957135616594,0.,-0.0092588838126317));
#4867=DIRECTION('ref_axis',(0.0092588838126317,-1.48029736616688E-15,-0.999957135616594));
#4868=DIRECTION('',(0.999957135616594,0.,0.00925888381263174));
#4869=DIRECTION('center_axis',(1.,0.,0.));
#4870=DIRECTION('ref_axis',(0.,-1.48023391413302E-15,-1.));
#4871=DIRECTION('center_axis',(-0.999957135616594,0.,-0.0092588838126317));
#4872=DIRECTION('ref_axis',(-0.00196997527928334,0.97710319176213,0.212756837365233));
#4873=DIRECTION('',(0.999957135616594,0.,0.00925888381263174));
#4874=DIRECTION('center_axis',(-1.,0.,0.));
#4875=DIRECTION('ref_axis',(0.,-1.55456280282127E-13,1.));
#4876=DIRECTION('center_axis',(-0.999957135616594,0.,-0.0092588838126317));
#4877=DIRECTION('ref_axis',(0.00196997527928333,-0.977103191762131,-0.212756837365232));
#4878=DIRECTION('',(0.999957135616594,0.,0.00925888381263174));
#4879=DIRECTION('center_axis',(1.,0.,0.));
#4880=DIRECTION('ref_axis',(0.,-3.29791490337855E-13,-1.));
#4881=DIRECTION('center_axis',(0.0092588838126317,0.,-0.999957135616594));
#4882=DIRECTION('ref_axis',(0.,-1.,0.));
#4883=DIRECTION('',(0.999957135616594,0.,0.0092588838126317));
#4884=DIRECTION('',(0.,1.,0.));
#4885=DIRECTION('center_axis',(0.999957135616594,0.,0.0092588838126317));
#4886=DIRECTION('ref_axis',(-0.00654701953012895,0.707106781186548,0.70707647149037));
#4887=DIRECTION('center_axis',(1.,0.,0.));
#4888=DIRECTION('ref_axis',(0.,8.99427132075075E-13,1.));
#4889=DIRECTION('center_axis',(-1.,0.,0.));
#4890=DIRECTION('ref_axis',(0.,0.,1.));
#4891=DIRECTION('',(0.,1.,0.));
#4892=DIRECTION('center_axis',(1.,0.,0.));
#4893=DIRECTION('ref_axis',(0.,1.,0.));
#4894=DIRECTION('center_axis',(-1.,0.,0.));
#4895=DIRECTION('ref_axis',(0.,1.,0.));
#4896=DIRECTION('center_axis',(-0.999957135616594,0.,-0.00925888381263175));
#4897=DIRECTION('ref_axis',(0.00925888381263175,0.,-0.999957135616594));
#4898=DIRECTION('center_axis',(-1.,0.,0.));
#4899=DIRECTION('ref_axis',(0.,1.,0.));
#4900=DIRECTION('',(-1.,0.,0.));
#4901=DIRECTION('center_axis',(1.,0.,0.));
#4902=DIRECTION('ref_axis',(0.,0.,-1.));
#4903=DIRECTION('',(0.,1.,0.));
#4904=DIRECTION('',(0.,1.,0.));
#4905=DIRECTION('center_axis',(0.,0.,-1.));
#4906=DIRECTION('ref_axis',(0.67202150503225,-0.740531631177352,0.));
#4907=DIRECTION('center_axis',(0.,0.,-1.));
#4908=DIRECTION('ref_axis',(0.67202150503225,-0.740531631177352,0.));
#4909=DIRECTION('center_axis',(-1.,0.,0.));
#4910=DIRECTION('ref_axis',(0.,-0.707106781186547,-0.707106781186548));
#4911=DIRECTION('',(-1.,0.,0.));
#4912=DIRECTION('center_axis',(0.,0.,1.));
#4913=DIRECTION('ref_axis',(1.,0.,0.));
#4914=DIRECTION('center_axis',(0.,0.,-1.));
#4915=DIRECTION('ref_axis',(1.,0.,0.));
#4916=DIRECTION('center_axis',(1.,0.,0.));
#4917=DIRECTION('ref_axis',(0.,0.707106781186547,-0.707106781186548));
#4918=DIRECTION('center_axis',(0.,0.,1.));
#4919=DIRECTION('ref_axis',(1.,0.,0.));
#4920=DIRECTION('',(0.,0.,-1.));
#4921=DIRECTION('center_axis',(0.,0.,-1.));
#4922=DIRECTION('ref_axis',(1.,0.,0.));
#4923=DIRECTION('center_axis',(0.,0.,1.));
#4924=DIRECTION('ref_axis',(1.,0.,0.));
#4925=DIRECTION('center_axis',(0.,0.,1.));
#4926=DIRECTION('ref_axis',(1.,0.,0.));
#4927=DIRECTION('center_axis',(0.,0.,1.));
#4928=DIRECTION('ref_axis',(1.,0.,0.));
#4929=DIRECTION('',(0.,0.,-1.));
#4930=DIRECTION('center_axis',(0.,0.,1.));
#4931=DIRECTION('ref_axis',(1.,0.,0.));
#4932=DIRECTION('',(0.,0.,-1.));
#4933=DIRECTION('center_axis',(0.,0.,-1.));
#4934=DIRECTION('ref_axis',(1.,0.,0.));
#4935=DIRECTION('center_axis',(0.,0.,1.));
#4936=DIRECTION('ref_axis',(1.,0.,0.));
#4937=DIRECTION('',(0.,0.,-1.));
#4938=DIRECTION('center_axis',(0.,1.,0.));
#4939=DIRECTION('ref_axis',(-1.,0.,0.));
#4940=DIRECTION('',(-0.00925888381263175,0.,0.999957135616594));
#4941=DIRECTION('center_axis',(1.,0.,0.));
#4942=DIRECTION('ref_axis',(0.,1.,0.));
#4943=DIRECTION('center_axis',(-1.,0.,0.));
#4944=DIRECTION('ref_axis',(0.,1.,0.));
#4945=DIRECTION('',(-0.866025403784439,0.5,-6.12323399573677E-17));
#4946=DIRECTION('center_axis',(-1.,0.,0.));
#4947=DIRECTION('ref_axis',(0.,1.,0.));
#4948=DIRECTION('',(-1.,0.,0.));
#4949=DIRECTION('center_axis',(1.,0.,0.));
#4950=DIRECTION('ref_axis',(0.,1.,0.));
#4951=DIRECTION('center_axis',(-1.,0.,0.));
#4952=DIRECTION('ref_axis',(0.,1.,0.));
#4953=DIRECTION('',(-0.866025403784439,0.5,-6.12323399573677E-17));
#4954=DIRECTION('center_axis',(-1.,0.,0.));
#4955=DIRECTION('ref_axis',(0.,1.,0.));
#4956=DIRECTION('',(-1.,0.,0.));
#4957=DIRECTION('center_axis',(0.,0.,1.));
#4958=DIRECTION('ref_axis',(1.,0.,0.));
#4959=DIRECTION('center_axis',(0.,0.,1.));
#4960=DIRECTION('ref_axis',(1.,0.,0.));
#4961=DIRECTION('',(0.,1.,0.));
#4962=DIRECTION('center_axis',(0.,1.,0.));
#4963=DIRECTION('ref_axis',(-1.,0.,5.07530525542928E-16));
#4964=DIRECTION('center_axis',(0.,0.,-1.));
#4965=DIRECTION('ref_axis',(-1.,0.,0.));
#4966=DIRECTION('',(0.,1.,0.));
#4967=DIRECTION('center_axis',(0.999957135616594,0.,0.00925888381263175));
#4968=DIRECTION('ref_axis',(0.00925888381263175,0.,-0.999957135616594));
#4969=DIRECTION('axis',(0.,0.,1.));
#4970=DIRECTION('refdir',(1.,0.,0.));
#4971=DIRECTION('center_axis',(1.,0.,0.));
#4972=DIRECTION('ref_axis',(0.,-1.,0.));
#4973=DIRECTION('center_axis',(1.,0.,0.));
#4974=DIRECTION('ref_axis',(0.,-1.,0.));
#4975=DIRECTION('',(1.,0.,0.));
#4976=DIRECTION('center_axis',(1.,0.,0.));
#4977=DIRECTION('ref_axis',(0.,-1.,0.));
#4978=DIRECTION('center_axis',(-1.,0.,0.));
#4979=DIRECTION('ref_axis',(0.,-1.,0.));
#4980=DIRECTION('center_axis',(1.,0.,0.));
#4981=DIRECTION('ref_axis',(0.,-1.,0.));
#4982=DIRECTION('center_axis',(1.,0.,0.));
#4983=DIRECTION('ref_axis',(0.,-1.,0.));
#4984=DIRECTION('',(1.,0.,0.));
#4985=DIRECTION('center_axis',(1.,0.,0.));
#4986=DIRECTION('ref_axis',(0.,-1.,0.));
#4987=DIRECTION('center_axis',(-1.,0.,0.));
#4988=DIRECTION('ref_axis',(0.,-1.,0.));
#4989=DIRECTION('',(-1.,0.,0.));
#4990=DIRECTION('center_axis',(-1.,0.,0.));
#4991=DIRECTION('ref_axis',(0.,-1.,0.));
#4992=DIRECTION('',(0.,1.,-2.53765262771464E-16));
#4993=DIRECTION('',(0.,2.02447305031589E-16,-1.));
#4994=DIRECTION('center_axis',(0.,-1.,2.53765262771464E-16));
#4995=DIRECTION('ref_axis',(0.707106781186548,1.79439138135289E-16,0.707106781186548));
#4996=DIRECTION('',(0.,1.,-2.53765262771464E-16));
#4997=DIRECTION('center_axis',(0.,-0.999999999997375,-2.2912420403343E-6));
#4998=DIRECTION('ref_axis',(0.,-2.2912420403343E-6,0.999999999997375));
#4999=DIRECTION('',(0.,-1.,2.53765262771464E-16));
#5000=DIRECTION('center_axis',(0.,1.,2.02447305031589E-16));
#5001=DIRECTION('ref_axis',(0.707106781186548,1.79439138135289E-16,0.707106781186548));
#5002=DIRECTION('center_axis',(-1.,0.,0.));
#5003=DIRECTION('ref_axis',(0.,-1.,0.));
#5004=DIRECTION('',(0.,-2.2912420403343E-6,0.999999999997375));
#5005=DIRECTION('center_axis',(0.,-1.,0.));
#5006=DIRECTION('ref_axis',(0.,0.,1.));
#5007=DIRECTION('',(-1.,0.,0.));
#5008=DIRECTION('center_axis',(0.,1.,0.));
#5009=DIRECTION('ref_axis',(5.92118946466749E-15,0.,-1.));
#5010=DIRECTION('',(-1.,0.,0.));
#5011=DIRECTION('',(-1.,0.,0.));
#5012=DIRECTION('center_axis',(-1.,0.,0.));
#5013=DIRECTION('ref_axis',(0.,5.15150041143406E-8,0.999999999999999));
#5014=DIRECTION('',(-1.,0.,0.));
#5015=DIRECTION('center_axis',(0.,5.15150011224698E-8,0.999999999999999));
#5016=DIRECTION('ref_axis',(0.,0.999999999999999,-5.15150011224698E-8));
#5017=DIRECTION('',(-1.,0.,0.));
#5018=DIRECTION('center_axis',(-1.,0.,0.));
#5019=DIRECTION('ref_axis',(0.,-9.9257750216751E-16,-1.));
#5020=DIRECTION('',(-1.,0.,0.));
#5021=DIRECTION('center_axis',(-1.,0.,0.));
#5022=DIRECTION('ref_axis',(0.,0.981911225094666,0.189341876068374));
#5023=DIRECTION('',(-1.,0.,0.));
#5024=DIRECTION('center_axis',(-1.,0.,0.));
#5025=DIRECTION('ref_axis',(0.,-0.981911225094667,-0.18934187606837));
#5026=DIRECTION('',(-1.,0.,0.));
#5027=DIRECTION('center_axis',(0.,-5.15150011224698E-8,0.999999999999999));
#5028=DIRECTION('ref_axis',(0.,0.999999999999999,5.15150011224698E-8));
#5029=DIRECTION('',(-1.,0.,0.));
#5030=DIRECTION('center_axis',(-1.,0.,0.));
#5031=DIRECTION('ref_axis',(0.,1.,-2.96059473233376E-15));
#5032=DIRECTION('',(-1.,0.,0.));
#5033=DIRECTION('center_axis',(1.,0.,0.));
#5034=DIRECTION('ref_axis',(0.,1.,-2.96059473233376E-15));
#5035=DIRECTION('',(1.,0.,0.));
#5036=DIRECTION('center_axis',(0.,1.,0.));
#5037=DIRECTION('ref_axis',(0.,0.,-1.));
#5038=DIRECTION('',(-1.,0.,0.));
#5039=DIRECTION('center_axis',(0.,-1.,0.));
#5040=DIRECTION('ref_axis',(5.92118946466749E-15,0.,-1.));
#5041=DIRECTION('',(0.,0.,1.));
#5042=DIRECTION('center_axis',(0.,0.,-1.));
#5043=DIRECTION('ref_axis',(0.,-1.,0.));
#5044=DIRECTION('',(0.,1.,0.));
#5045=DIRECTION('',(-1.,0.,0.));
#5046=DIRECTION('',(0.,1.,0.));
#5047=DIRECTION('center_axis',(0.,-1.,-2.02447305031589E-16));
#5048=DIRECTION('ref_axis',(0.,2.02447305031589E-16,-1.));
#5049=DIRECTION('',(1.,0.,0.));
#5050=DIRECTION('',(0.,2.02447305031589E-16,-1.));
#5051=DIRECTION('center_axis',(0.,2.53765262771464E-16,1.));
#5052=DIRECTION('ref_axis',(0.,-1.,2.53765262771464E-16));
#5053=DIRECTION('',(1.,0.,0.));
#5054=DIRECTION('',(0.,1.,-2.53765262771464E-16));
#5055=DIRECTION('center_axis',(0.,0.999999999997375,2.2912420403343E-6));
#5056=DIRECTION('ref_axis',(0.,-2.2912420403343E-6,0.999999999997375));
#5057=DIRECTION('',(0.,2.2912420403343E-6,-0.999999999997375));
#5058=DIRECTION('center_axis',(1.,0.,0.));
#5059=DIRECTION('ref_axis',(0.,0.,1.));
#5060=DIRECTION('',(0.,-1.,0.));
#5061=DIRECTION('center_axis',(0.,-1.,0.));
#5062=DIRECTION('ref_axis',(5.92118946466749E-15,0.,-1.));
#5063=DIRECTION('center_axis',(0.,-1.,0.));
#5064=DIRECTION('ref_axis',(5.92118946466749E-15,0.,-1.));
#5065=DIRECTION('',(0.,-1.,0.));
#5066=DIRECTION('center_axis',(0.,1.,0.));
#5067=DIRECTION('ref_axis',(5.92118946466749E-15,0.,-1.));
#5068=DIRECTION('',(0.,1.,0.));
#5069=DIRECTION('center_axis',(-3.9666966593473E-16,0.,-1.));
#5070=DIRECTION('ref_axis',(1.,0.,-3.9666966593473E-16));
#5071=DIRECTION('',(1.,0.,-3.9666966593473E-16));
#5072=DIRECTION('',(0.,-1.,0.));
#5073=DIRECTION('',(-1.,0.,3.9666966593473E-16));
#5074=DIRECTION('center_axis',(0.,-1.,0.));
#5075=DIRECTION('ref_axis',(2.96059473233377E-15,0.,1.));
#5076=DIRECTION('center_axis',(0.,1.,0.));
#5077=DIRECTION('ref_axis',(2.96059473233377E-15,0.,1.));
#5078=DIRECTION('',(0.,-1.,0.));
#5079=DIRECTION('center_axis',(0.,-1.,0.));
#5080=DIRECTION('ref_axis',(2.96059473233377E-15,0.,1.));
#5081=DIRECTION('center_axis',(0.965925826289068,0.,-0.258819045102521));
#5082=DIRECTION('ref_axis',(0.258819045102521,0.,0.965925826289068));
#5083=DIRECTION('',(0.258819045102521,0.,0.965925826289068));
#5084=DIRECTION('',(0.,1.,0.));
#5085=DIRECTION('',(0.258819045102521,0.,0.965925826289068));
#5086=DIRECTION('',(0.,-1.,0.));
#5087=DIRECTION('',(-0.258819045102521,0.,-0.965925826289068));
#5088=DIRECTION('',(0.,1.,0.));
#5089=DIRECTION('',(-0.258819045102521,0.,-0.965925826289068));
#5090=DIRECTION('center_axis',(0.,0.,-1.));
#5091=DIRECTION('ref_axis',(0.,-1.,0.));
#5092=DIRECTION('',(-1.,0.,0.));
#5093=DIRECTION('',(0.,-1.,0.));
#5094=DIRECTION('center_axis',(0.,-1.,0.));
#5095=DIRECTION('ref_axis',(0.,0.,1.));
#5096=DIRECTION('',(-1.,0.,0.));
#5097=DIRECTION('',(0.,0.,1.));
#5098=DIRECTION('center_axis',(0.,0.,-1.));
#5099=DIRECTION('ref_axis',(0.,-1.,0.));
#5100=DIRECTION('',(-1.,0.,0.));
#5101=DIRECTION('',(0.,-1.,0.));
#5102=DIRECTION('center_axis',(0.,-1.,0.));
#5103=DIRECTION('ref_axis',(0.,0.,1.));
#5104=DIRECTION('',(-1.,0.,0.));
#5105=DIRECTION('',(0.,0.,1.));
#5106=DIRECTION('center_axis',(1.,0.,0.));
#5107=DIRECTION('ref_axis',(0.,1.,0.));
#5108=DIRECTION('center_axis',(-1.,0.,0.));
#5109=DIRECTION('ref_axis',(0.,1.,0.));
#5110=DIRECTION('',(-0.642787609686539,0.766044443118978,-9.38133875270273E-17));
#5111=DIRECTION('center_axis',(-1.,0.,0.));
#5112=DIRECTION('ref_axis',(0.,1.,0.));
#5113=DIRECTION('center_axis',(-1.,0.,0.));
#5114=DIRECTION('ref_axis',(0.,1.,0.));
#5115=DIRECTION('',(-1.,0.,0.));
#5116=DIRECTION('center_axis',(-1.,0.,0.));
#5117=DIRECTION('ref_axis',(0.,1.,0.));
#5118=DIRECTION('center_axis',(-1.,0.,0.));
#5119=DIRECTION('ref_axis',(0.,1.,0.));
#5120=DIRECTION('',(-1.,0.,0.));
#5121=DIRECTION('center_axis',(-1.,0.,0.));
#5122=DIRECTION('ref_axis',(0.,1.,0.));
#5123=DIRECTION('center_axis',(-1.,0.,0.));
#5124=DIRECTION('ref_axis',(0.,1.,0.));
#5125=DIRECTION('center_axis',(0.,0.,-1.));
#5126=DIRECTION('ref_axis',(0.,-1.,0.));
#5127=DIRECTION('',(0.,1.,0.));
#5128=DIRECTION('',(-1.,0.,0.));
#5129=DIRECTION('',(0.,-1.,0.));
#5130=DIRECTION('',(-1.,0.,0.));
#5131=DIRECTION('center_axis',(0.,1.,0.));
#5132=DIRECTION('ref_axis',(0.,0.,-1.));
#5133=DIRECTION('',(0.,0.,1.));
#5134=DIRECTION('',(0.,0.,-1.));
#5135=DIRECTION('',(-1.,0.,0.));
#5136=DIRECTION('center_axis',(0.,0.,1.));
#5137=DIRECTION('ref_axis',(0.,1.,0.));
#5138=DIRECTION('',(-1.,0.,0.));
#5139=DIRECTION('',(0.,-1.,0.));
#5140=DIRECTION('',(0.,1.,0.));
#5141=DIRECTION('',(-1.,0.,0.));
#5142=DIRECTION('',(0.,1.,0.));
#5143=DIRECTION('center_axis',(0.,1.,0.));
#5144=DIRECTION('ref_axis',(0.,0.,-1.));
#5145=DIRECTION('',(-1.,0.,0.));
#5146=DIRECTION('',(0.,0.,1.));
#5147=DIRECTION('center_axis',(0.,0.,-1.));
#5148=DIRECTION('ref_axis',(0.,-1.,0.));
#5149=DIRECTION('',(-1.,0.,0.));
#5150=DIRECTION('',(0.,1.,0.));
#5151=DIRECTION('center_axis',(0.,1.,0.));
#5152=DIRECTION('ref_axis',(0.,0.,-1.));
#5153=DIRECTION('',(0.,0.,1.));
#5154=DIRECTION('center_axis',(0.,-1.,0.));
#5155=DIRECTION('ref_axis',(0.,0.,1.));
#5156=DIRECTION('',(0.,0.,1.));
#5157=DIRECTION('',(0.,0.,1.));
#5158=DIRECTION('center_axis',(1.,0.,0.));
#5159=DIRECTION('ref_axis',(0.,1.,0.));
#5160=DIRECTION('center_axis',(1.,0.,0.));
#5161=DIRECTION('ref_axis',(0.,1.,0.));
#5162=DIRECTION('axis',(0.,0.,1.));
#5163=DIRECTION('refdir',(1.,0.,0.));
#5164=DIRECTION('center_axis',(0.,0.,-1.));
#5165=DIRECTION('ref_axis',(1.,0.,0.));
#5166=DIRECTION('center_axis',(0.,0.,-1.));
#5167=DIRECTION('ref_axis',(1.,0.,0.));
#5168=DIRECTION('center_axis',(0.,0.,-1.));
#5169=DIRECTION('ref_axis',(1.,0.,0.));
#5170=DIRECTION('center_axis',(0.,0.,-1.));
#5171=DIRECTION('ref_axis',(1.,0.,0.));
#5172=DIRECTION('center_axis',(0.,0.,-1.));
#5173=DIRECTION('ref_axis',(1.,0.,0.));
#5174=DIRECTION('',(0.,0.,-1.));
#5175=DIRECTION('center_axis',(0.,0.,-1.));
#5176=DIRECTION('ref_axis',(1.,0.,0.));
#5177=DIRECTION('',(0.,0.,-1.));
#5178=DIRECTION('center_axis',(0.,0.,1.));
#5179=DIRECTION('ref_axis',(1.,0.,0.));
#5180=DIRECTION('center_axis',(0.,0.,-1.));
#5181=DIRECTION('ref_axis',(1.,0.,0.));
#5182=DIRECTION('center_axis',(0.,0.,-1.));
#5183=DIRECTION('ref_axis',(1.,0.,0.));
#5184=DIRECTION('center_axis',(0.,0.,-1.));
#5185=DIRECTION('ref_axis',(1.,0.,0.));
#5186=DIRECTION('center_axis',(0.,0.,-1.));
#5187=DIRECTION('ref_axis',(1.,0.,0.));
#5188=DIRECTION('center_axis',(0.,0.,-1.));
#5189=DIRECTION('ref_axis',(1.,0.,0.));
#5190=DIRECTION('',(0.,0.,-1.));
#5191=DIRECTION('center_axis',(0.,0.,-1.));
#5192=DIRECTION('ref_axis',(1.,0.,0.));
#5193=DIRECTION('',(0.,0.,-1.));
#5194=DIRECTION('center_axis',(0.,0.,1.));
#5195=DIRECTION('ref_axis',(1.,0.,0.));
#5196=DIRECTION('center_axis',(0.,0.,1.));
#5197=DIRECTION('ref_axis',(1.,0.,0.));
#5198=DIRECTION('',(-1.,0.,0.));
#5199=DIRECTION('',(0.,1.,0.));
#5200=DIRECTION('',(1.,0.,0.));
#5201=DIRECTION('',(0.,-1.,0.));
#5202=DIRECTION('center_axis',(-1.,0.,0.));
#5203=DIRECTION('ref_axis',(0.,-1.,0.));
#5204=DIRECTION('',(0.,0.,1.));
#5205=DIRECTION('',(0.,-1.,0.));
#5206=DIRECTION('',(0.,0.,1.));
#5207=DIRECTION('center_axis',(0.,1.,0.));
#5208=DIRECTION('ref_axis',(-1.,0.,0.));
#5209=DIRECTION('',(-1.,0.,0.));
#5210=DIRECTION('',(0.,0.,1.));
#5211=DIRECTION('center_axis',(1.,0.,0.));
#5212=DIRECTION('ref_axis',(0.,1.,0.));
#5213=DIRECTION('',(0.,1.,0.));
#5214=DIRECTION('',(0.,0.,1.));
#5215=DIRECTION('center_axis',(0.,-1.,0.));
#5216=DIRECTION('ref_axis',(1.,0.,0.));
#5217=DIRECTION('',(1.,0.,0.));
#5218=DIRECTION('center_axis',(0.,0.,1.));
#5219=DIRECTION('ref_axis',(1.,0.,0.));
#5220=DIRECTION('axis',(0.,0.,1.));
#5221=DIRECTION('refdir',(1.,0.,0.));
#5222=DIRECTION('center_axis',(-1.,0.,0.));
#5223=DIRECTION('ref_axis',(0.,0.,1.));
#5224=DIRECTION('center_axis',(-1.,0.,0.));
#5225=DIRECTION('ref_axis',(0.,1.,0.));
#5226=DIRECTION('center_axis',(0.,-1.,1.22464679914735E-16));
#5227=DIRECTION('ref_axis',(0.,-1.22464679914735E-16,-1.));
#5228=DIRECTION('center_axis',(1.,0.,0.));
#5229=DIRECTION('ref_axis',(0.,1.,0.));
#5230=DIRECTION('center_axis',(-1.,0.,0.));
#5231=DIRECTION('ref_axis',(0.,1.,0.));
#5232=DIRECTION('center_axis',(1.,0.,0.));
#5233=DIRECTION('ref_axis',(0.,1.,0.));
#5234=DIRECTION('center_axis',(1.,0.,0.));
#5235=DIRECTION('ref_axis',(0.,1.,0.));
#5236=DIRECTION('',(-1.,0.,0.));
#5237=DIRECTION('center_axis',(1.,0.,0.));
#5238=DIRECTION('ref_axis',(0.,1.,0.));
#5239=DIRECTION('center_axis',(1.,0.,0.));
#5240=DIRECTION('ref_axis',(0.,1.,0.));
#5241=DIRECTION('center_axis',(0.,-0.5,-0.866025403784439));
#5242=DIRECTION('ref_axis',(0.,0.866025403784439,-0.5));
#5243=DIRECTION('',(0.,0.866025403784439,-0.5));
#5244=DIRECTION('',(1.,0.,0.));
#5245=DIRECTION('',(0.,0.866025403784439,-0.5));
#5246=DIRECTION('',(1.,0.,0.));
#5247=DIRECTION('center_axis',(0.,-1.,-1.58603286868792E-16));
#5248=DIRECTION('ref_axis',(0.,1.58603286868792E-16,-1.));
#5249=DIRECTION('',(0.,1.58603286868792E-16,-1.));
#5250=DIRECTION('',(1.,0.,0.));
#5251=DIRECTION('',(0.,1.58603286868792E-16,-1.));
#5252=DIRECTION('center_axis',(0.,-0.5,0.866025403784439));
#5253=DIRECTION('ref_axis',(0.,-0.866025403784439,-0.5));
#5254=DIRECTION('',(0.,-0.866025403784439,-0.5));
#5255=DIRECTION('',(1.,0.,0.));
#5256=DIRECTION('',(0.,-0.866025403784439,-0.5));
#5257=DIRECTION('center_axis',(0.,0.5,0.866025403784439));
#5258=DIRECTION('ref_axis',(0.,-0.866025403784439,0.5));
#5259=DIRECTION('',(0.,-0.866025403784439,0.5));
#5260=DIRECTION('',(1.,0.,0.));
#5261=DIRECTION('',(0.,-0.866025403784439,0.5));
#5262=DIRECTION('center_axis',(0.,1.,3.17206573737584E-16));
#5263=DIRECTION('ref_axis',(0.,-3.17206573737584E-16,1.));
#5264=DIRECTION('',(0.,-3.17206573737584E-16,1.));
#5265=DIRECTION('',(1.,0.,0.));
#5266=DIRECTION('',(0.,-3.17206573737584E-16,1.));
#5267=DIRECTION('center_axis',(0.,0.5,-0.866025403784439));
#5268=DIRECTION('ref_axis',(0.,0.866025403784439,0.5));
#5269=DIRECTION('',(0.,0.866025403784439,0.5));
#5270=DIRECTION('',(0.,0.866025403784439,0.5));
#5271=DIRECTION('center_axis',(1.,0.,0.));
#5272=DIRECTION('ref_axis',(0.,0.,-1.));
#5273=DIRECTION('center_axis',(-1.,0.,0.));
#5274=DIRECTION('ref_axis',(0.,0.,1.));
#5275=DIRECTION('center_axis',(1.,0.,0.));
#5276=DIRECTION('ref_axis',(0.,1.,0.));
#5277=DIRECTION('center_axis',(0.,-1.,1.22464679914735E-16));
#5278=DIRECTION('ref_axis',(0.,-1.22464679914735E-16,-1.));
#5279=DIRECTION('center_axis',(-1.,0.,0.));
#5280=DIRECTION('ref_axis',(0.,1.,0.));
#5281=DIRECTION('center_axis',(-1.,0.,0.));
#5282=DIRECTION('ref_axis',(0.,1.,0.));
#5283=DIRECTION('center_axis',(-1.,0.,0.));
#5284=DIRECTION('ref_axis',(0.,1.,0.));
#5285=DIRECTION('',(1.,0.,0.));
#5286=DIRECTION('center_axis',(1.,0.,0.));
#5287=DIRECTION('ref_axis',(0.,1.,0.));
#5288=DIRECTION('center_axis',(1.,0.,0.));
#5289=DIRECTION('ref_axis',(0.,1.,0.));
#5290=DIRECTION('axis',(0.,0.,1.));
#5291=DIRECTION('refdir',(1.,0.,0.));
#5292=DIRECTION('center_axis',(-1.,0.,0.));
#5293=DIRECTION('ref_axis',(0.,-1.,0.));
#5294=DIRECTION('center_axis',(1.,0.,0.));
#5295=DIRECTION('ref_axis',(0.,1.,0.));
#5296=DIRECTION('',(0.,0.,1.));
#5297=DIRECTION('center_axis',(-1.,0.,0.));
#5298=DIRECTION('ref_axis',(0.,1.,0.));
#5299=DIRECTION('',(0.,0.,1.));
#5300=DIRECTION('center_axis',(0.,1.,0.));
#5301=DIRECTION('ref_axis',(-1.,0.,0.));
#5302=DIRECTION('',(-1.,0.,0.));
#5303=DIRECTION('',(0.,0.,-1.));
#5304=DIRECTION('',(1.,0.,0.));
#5305=DIRECTION('center_axis',(0.,1.,0.));
#5306=DIRECTION('ref_axis',(-1.,0.,0.));
#5307=DIRECTION('',(1.,0.,0.));
#5308=DIRECTION('',(0.,0.,1.));
#5309=DIRECTION('',(-1.,0.,0.));
#5310=DIRECTION('',(0.,0.,-1.));
#5311=DIRECTION('center_axis',(-4.20539024479226E-17,-1.,0.));
#5312=DIRECTION('ref_axis',(1.,-4.20539024479226E-17,0.));
#5313=DIRECTION('',(1.,0.,0.));
#5314=DIRECTION('',(-1.,0.,0.));
#5315=DIRECTION('',(0.,0.,1.));
#5316=DIRECTION('center_axis',(-4.20539024479226E-17,-1.,0.));
#5317=DIRECTION('ref_axis',(1.,-4.20539024479226E-17,0.));
#5318=DIRECTION('',(-1.,0.,0.));
#5319=DIRECTION('',(0.,0.,1.));
#5320=DIRECTION('',(1.,0.,0.));
#5321=DIRECTION('',(0.,0.,1.));
#5322=DIRECTION('center_axis',(-1.,0.,0.));
#5323=DIRECTION('ref_axis',(0.,-1.,0.));
#5324=DIRECTION('center_axis',(1.,0.,0.));
#5325=DIRECTION('ref_axis',(0.,1.,0.));
#5326=DIRECTION('center_axis',(-1.,0.,0.));
#5327=DIRECTION('ref_axis',(0.,1.,0.));
#5328=DIRECTION('center_axis',(1.,0.,0.));
#5329=DIRECTION('ref_axis',(0.,1.,0.));
#5330=DIRECTION('center_axis',(-1.,0.,0.));
#5331=DIRECTION('ref_axis',(0.,1.,0.));
#5332=DIRECTION('center_axis',(-1.,0.,0.));
#5333=DIRECTION('ref_axis',(0.,1.,0.));
#5334=DIRECTION('center_axis',(1.,0.,0.));
#5335=DIRECTION('ref_axis',(0.,1.,0.));
#5336=DIRECTION('center_axis',(1.,0.,0.));
#5337=DIRECTION('ref_axis',(0.,1.,0.));
#5338=DIRECTION('center_axis',(1.,0.,0.));
#5339=DIRECTION('ref_axis',(0.,1.,0.));
#5340=DIRECTION('center_axis',(1.,0.,0.));
#5341=DIRECTION('ref_axis',(0.,1.,0.));
#5342=DIRECTION('center_axis',(-1.,0.,0.));
#5343=DIRECTION('ref_axis',(0.,1.,0.));
#5344=DIRECTION('center_axis',(1.,0.,0.));
#5345=DIRECTION('ref_axis',(0.,1.,0.));
#5346=DIRECTION('',(-1.,0.,0.));
#5347=DIRECTION('center_axis',(1.,0.,0.));
#5348=DIRECTION('ref_axis',(0.,1.,0.));
#5349=DIRECTION('center_axis',(-1.,0.,0.));
#5350=DIRECTION('ref_axis',(0.,1.,0.));
#5351=DIRECTION('',(-1.,0.,0.));
#5352=DIRECTION('center_axis',(1.,0.,0.));
#5353=DIRECTION('ref_axis',(0.,1.,0.));
#5354=DIRECTION('center_axis',(1.,0.,0.));
#5355=DIRECTION('ref_axis',(0.,1.,0.));
#5356=DIRECTION('axis',(0.,0.,1.));
#5357=DIRECTION('refdir',(1.,0.,0.));
#5358=DIRECTION('center_axis',(0.,0.,1.));
#5359=DIRECTION('ref_axis',(1.,0.,0.));
#5360=DIRECTION('center_axis',(0.,0.,-1.));
#5361=DIRECTION('ref_axis',(1.,0.,0.));
#5362=DIRECTION('',(0.,0.,-1.));
#5363=DIRECTION('center_axis',(0.,0.,-1.));
#5364=DIRECTION('ref_axis',(1.,0.,0.));
#5365=DIRECTION('center_axis',(0.,0.,1.));
#5366=DIRECTION('ref_axis',(0.,1.,0.));
#5367=DIRECTION('center_axis',(0.,0.,1.));
#5368=DIRECTION('ref_axis',(0.,1.,0.));
#5369=DIRECTION('',(0.,0.,1.));
#5370=DIRECTION('center_axis',(0.,0.,-1.));
#5371=DIRECTION('ref_axis',(0.,1.,0.));
#5372=DIRECTION('',(0.,0.,1.));
#5373=DIRECTION('center_axis',(0.,1.,0.));
#5374=DIRECTION('ref_axis',(-1.,0.,0.));
#5375=DIRECTION('',(1.,0.,0.));
#5376=DIRECTION('',(-1.,0.,0.));
#5377=DIRECTION('',(0.,0.,1.));
#5378=DIRECTION('center_axis',(0.,0.,1.));
#5379=DIRECTION('ref_axis',(0.90350790038088,-0.428571433893271,0.));
#5380=DIRECTION('center_axis',(0.,0.,1.));
#5381=DIRECTION('ref_axis',(0.90350790038088,-0.428571433893271,0.));
#5382=DIRECTION('center_axis',(0.,0.,1.));
#5383=DIRECTION('ref_axis',(0.90350790038088,-0.428571433893271,0.));
#5384=DIRECTION('',(0.,0.,1.));
#5385=DIRECTION('center_axis',(0.,0.,1.));
#5386=DIRECTION('ref_axis',(-1.,-2.96059473233375E-16,0.));
#5387=DIRECTION('center_axis',(0.,0.,1.));
#5388=DIRECTION('ref_axis',(0.903507900380879,0.428571433893272,0.));
#5389=DIRECTION('center_axis',(0.,0.,1.));
#5390=DIRECTION('ref_axis',(0.903507900380879,0.428571433893272,0.));
#5391=DIRECTION('',(0.,0.,1.));
#5392=DIRECTION('center_axis',(0.,0.,1.));
#5393=DIRECTION('ref_axis',(0.,-1.,0.));
#5394=DIRECTION('center_axis',(0.,0.,1.));
#5395=DIRECTION('ref_axis',(0.,-1.,0.));
#5396=DIRECTION('center_axis',(0.,0.,1.));
#5397=DIRECTION('ref_axis',(0.,-1.,0.));
#5398=DIRECTION('',(0.,0.,1.));
#5399=DIRECTION('center_axis',(0.,-1.,0.));
#5400=DIRECTION('ref_axis',(1.,0.,0.));
#5401=DIRECTION('',(1.,0.,0.));
#5402=DIRECTION('',(1.,0.,0.));
#5403=DIRECTION('center_axis',(0.,0.,1.));
#5404=DIRECTION('ref_axis',(1.,0.,0.));
#5405=DIRECTION('center_axis',(0.,0.,1.));
#5406=DIRECTION('ref_axis',(1.,0.,0.));
#5407=DIRECTION('axis',(0.,0.,1.));
#5408=DIRECTION('refdir',(1.,0.,0.));
#5409=DIRECTION('center_axis',(0.,1.,0.));
#5410=DIRECTION('ref_axis',(0.,0.,1.));
#5411=DIRECTION('',(0.,0.,1.));
#5412=DIRECTION('',(-1.,0.,0.));
#5413=DIRECTION('',(0.,0.,1.));
#5414=DIRECTION('',(1.,0.,0.));
#5415=DIRECTION('center_axis',(0.,-1.,0.));
#5416=DIRECTION('ref_axis',(0.,0.,-1.));
#5417=DIRECTION('',(0.,0.,-1.));
#5418=DIRECTION('',(-1.,0.,0.));
#5419=DIRECTION('',(0.,0.,-1.));
#5420=DIRECTION('',(1.,0.,0.));
#5421=DIRECTION('center_axis',(-1.,0.,0.));
#5422=DIRECTION('ref_axis',(0.,-1.,0.));
#5423=DIRECTION('center_axis',(1.,0.,0.));
#5424=DIRECTION('ref_axis',(0.,1.,0.));
#5425=DIRECTION('center_axis',(1.,0.,0.));
#5426=DIRECTION('ref_axis',(0.,1.,0.));
#5427=DIRECTION('center_axis',(1.,0.,0.));
#5428=DIRECTION('ref_axis',(0.,1.,0.));
#5429=DIRECTION('center_axis',(1.,0.,0.));
#5430=DIRECTION('ref_axis',(0.,1.,0.));
#5431=DIRECTION('center_axis',(1.,0.,0.));
#5432=DIRECTION('ref_axis',(0.,1.,0.));
#5433=DIRECTION('center_axis',(1.,0.,0.));
#5434=DIRECTION('ref_axis',(0.,1.,0.));
#5435=DIRECTION('center_axis',(1.,0.,0.));
#5436=DIRECTION('ref_axis',(0.,1.,0.));
#5437=DIRECTION('center_axis',(1.,0.,0.));
#5438=DIRECTION('ref_axis',(0.,1.,0.));
#5439=DIRECTION('center_axis',(1.,0.,0.));
#5440=DIRECTION('ref_axis',(0.,1.,0.));
#5441=DIRECTION('',(-1.,0.,0.));
#5442=DIRECTION('center_axis',(-1.,0.,0.));
#5443=DIRECTION('ref_axis',(0.,1.,0.));
#5444=DIRECTION('center_axis',(1.,0.,0.));
#5445=DIRECTION('ref_axis',(0.,1.,0.));
#5446=DIRECTION('center_axis',(1.,0.,0.));
#5447=DIRECTION('ref_axis',(0.,1.,0.));
#5448=DIRECTION('center_axis',(1.,0.,0.));
#5449=DIRECTION('ref_axis',(0.,1.,0.));
#5450=DIRECTION('',(-1.,0.,0.));
#5451=DIRECTION('center_axis',(1.,0.,0.));
#5452=DIRECTION('ref_axis',(0.,1.,0.));
#5453=DIRECTION('axis',(0.,0.,1.));
#5454=DIRECTION('refdir',(1.,0.,0.));
#5455=DIRECTION('center_axis',(-1.,0.,0.));
#5456=DIRECTION('ref_axis',(0.,0.,1.));
#5457=DIRECTION('center_axis',(1.,0.,0.));
#5458=DIRECTION('ref_axis',(0.,-1.,0.));
#5459=DIRECTION('center_axis',(0.,-1.,1.22464679914735E-16));
#5460=DIRECTION('ref_axis',(0.,-1.22464679914735E-16,-1.));
#5461=DIRECTION('center_axis',(-1.,0.,0.));
#5462=DIRECTION('ref_axis',(0.,-1.,0.));
#5463=DIRECTION('center_axis',(-1.,0.,0.));
#5464=DIRECTION('ref_axis',(0.,-1.,0.));
#5465=DIRECTION('center_axis',(-1.,0.,0.));
#5466=DIRECTION('ref_axis',(0.,-1.,0.));
#5467=DIRECTION('',(1.,0.,0.));
#5468=DIRECTION('center_axis',(-1.,0.,0.));
#5469=DIRECTION('ref_axis',(0.,-1.,0.));
#5470=DIRECTION('center_axis',(-1.,0.,0.));
#5471=DIRECTION('ref_axis',(0.,-1.,0.));
#5472=DIRECTION('center_axis',(-1.,0.,0.));
#5473=DIRECTION('ref_axis',(0.,-1.,0.));
#5474=DIRECTION('center_axis',(1.,0.,0.));
#5475=DIRECTION('ref_axis',(0.,0.,-1.));
#5476=DIRECTION('center_axis',(1.,0.,0.));
#5477=DIRECTION('ref_axis',(0.,-1.,0.));
#5478=DIRECTION('center_axis',(1.,0.,0.));
#5479=DIRECTION('ref_axis',(0.,-1.,0.));
#5480=DIRECTION('center_axis',(0.,1.,1.22464679914735E-16));
#5481=DIRECTION('ref_axis',(0.,-1.22464679914735E-16,1.));
#5482=DIRECTION('center_axis',(-1.,0.,0.));
#5483=DIRECTION('ref_axis',(0.,-1.,0.));
#5484=DIRECTION('',(1.,0.,0.));
#5485=DIRECTION('center_axis',(-1.,0.,0.));
#5486=DIRECTION('ref_axis',(0.,-1.,0.));
#5487=DIRECTION('center_axis',(-1.,0.,0.));
#5488=DIRECTION('ref_axis',(0.,-1.,0.));
#5489=DIRECTION('center_axis',(-1.,0.,0.));
#5490=DIRECTION('ref_axis',(0.,-1.,0.));
#5491=DIRECTION('center_axis',(-1.,0.,0.));
#5492=DIRECTION('ref_axis',(0.,-1.,0.));
#5493=DIRECTION('',(1.,0.,0.));
#5494=DIRECTION('center_axis',(1.,0.,0.));
#5495=DIRECTION('ref_axis',(0.,-1.,0.));
#5496=DIRECTION('center_axis',(1.,0.,0.));
#5497=DIRECTION('ref_axis',(0.,1.,0.));
#5498=DIRECTION('center_axis',(1.,0.,0.));
#5499=DIRECTION('ref_axis',(0.,1.,0.));
#5500=DIRECTION('center_axis',(1.,0.,0.));
#5501=DIRECTION('ref_axis',(0.,1.,0.));
#5502=DIRECTION('center_axis',(1.,0.,0.));
#5503=DIRECTION('ref_axis',(0.,1.,0.));
#5504=DIRECTION('center_axis',(1.,0.,0.));
#5505=DIRECTION('ref_axis',(0.,1.,0.));
#5506=DIRECTION('',(-1.,0.,0.));
#5507=DIRECTION('center_axis',(1.,0.,0.));
#5508=DIRECTION('ref_axis',(0.,1.,0.));
#5509=DIRECTION('center_axis',(1.,0.,0.));
#5510=DIRECTION('ref_axis',(0.,1.,0.));
#5511=DIRECTION('',(-1.,0.,0.));
#5512=DIRECTION('center_axis',(-1.,0.,0.));
#5513=DIRECTION('ref_axis',(0.,1.,0.));
#5514=DIRECTION('center_axis',(1.,0.,0.));
#5515=DIRECTION('ref_axis',(0.,1.,0.));
#5516=DIRECTION('center_axis',(1.,0.,0.));
#5517=DIRECTION('ref_axis',(0.,1.,0.));
#5518=DIRECTION('',(-1.,0.,0.));
#5519=DIRECTION('center_axis',(-1.,0.,0.));
#5520=DIRECTION('ref_axis',(0.,1.,0.));
#5521=DIRECTION('center_axis',(1.,0.,0.));
#5522=DIRECTION('ref_axis',(0.,1.,0.));
#5523=DIRECTION('center_axis',(1.,0.,0.));
#5524=DIRECTION('ref_axis',(0.,1.,0.));
#5525=DIRECTION('center_axis',(1.,0.,0.));
#5526=DIRECTION('ref_axis',(0.,1.,0.));
#5527=DIRECTION('',(-1.,0.,0.));
#5528=DIRECTION('center_axis',(1.,0.,0.));
#5529=DIRECTION('ref_axis',(0.,1.,0.));
#5530=DIRECTION('center_axis',(1.,0.,0.));
#5531=DIRECTION('ref_axis',(0.,1.,0.));
#5532=DIRECTION('center_axis',(1.,0.,0.));
#5533=DIRECTION('ref_axis',(0.,1.,0.));
#5534=DIRECTION('axis',(0.,0.,1.));
#5535=DIRECTION('refdir',(1.,0.,0.));
#5536=DIRECTION('center_axis',(1.,0.,0.));
#5537=DIRECTION('ref_axis',(0.,1.,0.));
#5538=DIRECTION('',(0.,-1.,0.));
#5539=DIRECTION('',(0.,0.,1.));
#5540=DIRECTION('',(0.,1.,0.));
#5541=DIRECTION('',(0.,0.,1.));
#5542=DIRECTION('center_axis',(0.,-1.,0.));
#5543=DIRECTION('ref_axis',(1.,0.,0.));
#5544=DIRECTION('',(1.,0.,0.));
#5545=DIRECTION('',(1.,0.,0.));
#5546=DIRECTION('',(0.,0.,1.));
#5547=DIRECTION('center_axis',(-1.,0.,0.));
#5548=DIRECTION('ref_axis',(0.,-1.,0.));
#5549=DIRECTION('',(0.,-1.,0.));
#5550=DIRECTION('',(0.,-1.,0.));
#5551=DIRECTION('',(0.,0.,1.));
#5552=DIRECTION('center_axis',(0.,1.,0.));
#5553=DIRECTION('ref_axis',(-1.,0.,0.));
#5554=DIRECTION('',(-1.,0.,0.));
#5555=DIRECTION('',(-1.,0.,0.));
#5556=DIRECTION('',(0.,0.,1.));
#5557=DIRECTION('center_axis',(1.,0.,0.));
#5558=DIRECTION('ref_axis',(0.,1.,0.));
#5559=DIRECTION('',(0.,1.,0.));
#5560=DIRECTION('',(0.,1.,0.));
#5561=DIRECTION('',(0.,0.,1.));
#5562=DIRECTION('center_axis',(0.,-1.,0.));
#5563=DIRECTION('ref_axis',(1.,0.,0.));
#5564=DIRECTION('',(1.,0.,0.));
#5565=DIRECTION('',(1.,0.,0.));
#5566=DIRECTION('',(0.,0.,1.));
#5567=DIRECTION('center_axis',(-1.,0.,0.));
#5568=DIRECTION('ref_axis',(0.,-1.,0.));
#5569=DIRECTION('',(0.,-1.,0.));
#5570=DIRECTION('',(0.,-1.,0.));
#5571=DIRECTION('',(0.,0.,1.));
#5572=DIRECTION('center_axis',(0.,-1.,0.));
#5573=DIRECTION('ref_axis',(1.,0.,0.));
#5574=DIRECTION('',(1.,0.,0.));
#5575=DIRECTION('',(1.,0.,0.));
#5576=DIRECTION('center_axis',(0.,0.,1.));
#5577=DIRECTION('ref_axis',(1.,0.,0.));
#5578=DIRECTION('center_axis',(0.,0.,1.));
#5579=DIRECTION('ref_axis',(1.,0.,0.));
#5580=DIRECTION('',(0.,0.,1.));
#5581=DIRECTION('',(1.,0.,0.));
#5582=DIRECTION('',(1.,-8.32667268469117E-17,1.57772181044202E-30));
#5583=DIRECTION('',(1.24900090270425E-16,1.,-8.59035065303716E-15));
#5584=DIRECTION('',(1.38401432086199E-16,-0.365014182299005,-0.931001958494497));
#5585=DIRECTION('',(-1.,5.17029307199153E-15,-1.14727130907259E-15));
#5586=DIRECTION('',(-9.86076131526265E-32,0.,-1.));
#5587=DIRECTION('',(-1.,0.,9.86076131526265E-32));
#5588=DIRECTION('',(-3.94430452610506E-31,0.,0.999999999999981));
#5589=DIRECTION('',(0.999999999999994,0.,3.94430452610511E-31));
#5590=DIRECTION('',(-1.,2.2204460492504E-16,0.));
#5591=DIRECTION('',(-2.2204460492504E-16,-1.,-2.19269047363468E-15));
#5592=DIRECTION('',(0.,0.,1.));
#5593=DIRECTION('',(1.,0.,0.));
#5594=DIRECTION('',(0.,0.,1.));
#5595=DIRECTION('',(1.,0.,0.));
#5596=DIRECTION('',(0.,0.,1.));
#5597=DIRECTION('',(1.,0.,0.));
#5598=DIRECTION('',(1.,2.08166817117217E-15,1.08699486061216E-30));
#5599=DIRECTION('',(-2.08166817117217E-15,1.,-6.93889390390727E-17));
#5600=DIRECTION('',(1.26217744835362E-29,-6.66468057255202E-29,-1.));
#5601=DIRECTION('',(-1.,-2.13376789582852E-42,-1.26217744835362E-29));
#5602=DIRECTION('',(-2.93511883622906E-14,-0.98216120628523,0.188040859571361));
#5603=DIRECTION('',(-0.999999999999996,3.05586583598456E-14,0.));
#5604=DIRECTION('',(0.,-1.,0.));
#5605=DIRECTION('',(1.,0.,0.));
#5606=CARTESIAN_POINT('',(0.,0.,0.));
#5607=CARTESIAN_POINT('',(0.,0.,0.));
#5608=CARTESIAN_POINT('Origin',(183.750010137059,-16.,26.9988426616481));
#5609=CARTESIAN_POINT('',(0.,-12.5,25.2974497380605));
#5610=CARTESIAN_POINT('',(0.,-16.,25.2974497380605));
#5611=CARTESIAN_POINT('',(0.,-8.,25.2974497380605));
#5612=CARTESIAN_POINT('',(183.750010137059,-12.5,26.9988426616481));
#5613=CARTESIAN_POINT('',(183.750010137059,-12.5,26.9988426616481));
#5614=CARTESIAN_POINT('',(183.750010137059,-16.,26.9988426616481));
#5615=CARTESIAN_POINT('',(183.750010137059,-8.,26.9988426616481));
#5616=CARTESIAN_POINT('',(183.750010137059,-16.,26.9988426616481));
#5617=CARTESIAN_POINT('Origin',(184.,-16.,0.));
#5618=CARTESIAN_POINT('',(0.,-16.,0.));
#5619=CARTESIAN_POINT('',(0.,-16.,0.));
#5620=CARTESIAN_POINT('',(184.,-16.,8.32667268468867E-16));
#5621=CARTESIAN_POINT('',(183.73612181134,-16.,28.4987783650729));
#5622=CARTESIAN_POINT('',(184.,-16.,0.));
#5623=CARTESIAN_POINT('Origin',(183.750010137059,16.,26.9988426616481));
#5624=CARTESIAN_POINT('',(184.,16.,8.32667268468867E-16));
#5625=CARTESIAN_POINT('',(0.,16.,0.));
#5626=CARTESIAN_POINT('',(183.87500506853,16.,0.));
#5627=CARTESIAN_POINT('',(183.750010137059,16.,26.9988426616481));
#5628=CARTESIAN_POINT('',(183.611126879869,16.,41.998199695897));
#5629=CARTESIAN_POINT('',(0.,16.,25.2974497380605));
#5630=CARTESIAN_POINT('',(183.750010137059,16.,26.9988426616481));
#5631=CARTESIAN_POINT('',(0.,16.,13.499421330824));
#5632=CARTESIAN_POINT('Origin',(183.601867996057,-12.5,42.9981568315136));
#5633=CARTESIAN_POINT('',(158.47224362268,12.5,42.7654745854044));
#5634=CARTESIAN_POINT('',(158.47224362268,-12.5,42.7654745854044));
#5635=CARTESIAN_POINT('',(158.47224362268,-6.25,42.7654745854044));
#5636=CARTESIAN_POINT('',(183.601867996057,12.5,42.9981568315136));
#5637=CARTESIAN_POINT('',(183.601867996057,12.5,42.9981568315136));
#5638=CARTESIAN_POINT('',(183.601867996057,-12.5,42.9981568315136));
#5639=CARTESIAN_POINT('',(183.601867996057,-6.25,42.9981568315136));
#5640=CARTESIAN_POINT('',(183.601867996057,-12.5,42.9981568315136));
#5641=CARTESIAN_POINT('Origin',(183.750010137059,-12.5,26.9988426616481));
#5642=CARTESIAN_POINT('',(0.,-12.5,41.298135597594));
#5643=CARTESIAN_POINT('',(0.,-12.5,13.499421330824));
#5644=CARTESIAN_POINT('',(31.47224362268,-12.5,41.5895459357437));
#5645=CARTESIAN_POINT('',(183.601867996057,-12.5,42.9981568315136));
#5646=CARTESIAN_POINT('',(31.47224362268,-12.5,37.));
#5647=CARTESIAN_POINT('',(31.47224362268,-12.5,54.499421330824));
#5648=CARTESIAN_POINT('',(158.47224362268,-12.5,37.));
#5649=CARTESIAN_POINT('',(107.61112687987,-12.5,37.));
#5650=CARTESIAN_POINT('',(158.47224362268,-12.5,31.999421330824));
#5651=CARTESIAN_POINT('',(183.611126879869,-12.5,41.998199695897));
#5652=CARTESIAN_POINT('Origin',(183.750010137059,12.5,26.9988426616481));
#5653=CARTESIAN_POINT('',(0.,12.5,25.2974497380605));
#5654=CARTESIAN_POINT('',(0.,6.25,25.2974497380605));
#5655=CARTESIAN_POINT('',(183.750010137059,12.5,26.9988426616481));
#5656=CARTESIAN_POINT('',(183.750010137059,6.25,26.9988426616481));
#5657=CARTESIAN_POINT('',(183.750010137059,12.5,26.9988426616481));
#5658=CARTESIAN_POINT('Origin',(183.601867996057,12.5,42.9981568315136));
#5659=CARTESIAN_POINT('',(0.,12.5,41.298135597594));
#5660=CARTESIAN_POINT('',(0.,12.5,21.4990784157568));
#5661=CARTESIAN_POINT('',(183.537055809368,12.5,49.9978567808297));
#5662=CARTESIAN_POINT('',(158.47224362268,12.5,37.));
#5663=CARTESIAN_POINT('',(158.47224362268,12.5,39.9990784157568));
#5664=CARTESIAN_POINT('',(31.47224362268,12.5,37.));
#5665=CARTESIAN_POINT('',(107.537055809368,12.5,37.));
#5666=CARTESIAN_POINT('',(31.47224362268,12.5,41.5895459357437));
#5667=CARTESIAN_POINT('',(31.47224362268,12.5,62.4990784157568));
#5668=CARTESIAN_POINT('',(183.601867996057,12.5,42.9981568315136));
#5669=CARTESIAN_POINT('Origin',(183.601867996057,-12.5,42.9981568315136));
#5670=CARTESIAN_POINT('',(0.,-6.25,41.2981355975939));
#5671=CARTESIAN_POINT('',(31.47224362268,-6.25,41.5895459357437));
#5672=CARTESIAN_POINT('Origin',(31.47224362268,0.,82.));
#5673=CARTESIAN_POINT('',(31.47224362268,35.,37.));
#5674=CARTESIAN_POINT('',(31.47224362268,0.,37.));
#5675=CARTESIAN_POINT('',(31.47224362268,35.,82.));
#5676=CARTESIAN_POINT('',(31.47224362268,35.,37.));
#5677=CARTESIAN_POINT('',(31.47224362268,-35.,82.));
#5678=CARTESIAN_POINT('',(31.47224362268,0.,82.));
#5679=CARTESIAN_POINT('',(31.47224362268,-35.,37.));
#5680=CARTESIAN_POINT('',(31.47224362268,-35.,37.));
#5681=CARTESIAN_POINT('',(31.47224362268,0.,37.));
#5682=CARTESIAN_POINT('',(31.47224362268,-22.,62.));
#5683=CARTESIAN_POINT('Origin',(31.47224362268,-19.,62.));
#5684=CARTESIAN_POINT('',(31.47224362268,16.,62.));
#5685=CARTESIAN_POINT('Origin',(31.47224362268,19.,62.));
#5686=CARTESIAN_POINT('Origin',(31.47224362268,0.,37.));
#5687=CARTESIAN_POINT('',(158.47224362268,35.,37.));
#5688=CARTESIAN_POINT('',(158.47224362268,0.,37.));
#5689=CARTESIAN_POINT('',(158.47224362268,35.,37.));
#5690=CARTESIAN_POINT('Origin',(0.,0.,0.));
#5691=CARTESIAN_POINT('',(0.,-35.,0.));
#5692=CARTESIAN_POINT('',(0.,0.,0.));
#5693=CARTESIAN_POINT('',(5.35595873207839E-16,-34.9999999999999,5.80384757729347));
#5694=CARTESIAN_POINT('',(0.,-35.,0.));
#5695=CARTESIAN_POINT('',(0.,-32.,11.));
#5696=CARTESIAN_POINT('Origin',(0.,-38.,11.));
#5697=CARTESIAN_POINT('',(0.,-32.,52.));
#5698=CARTESIAN_POINT('',(0.,-32.,20.5));
#5699=CARTESIAN_POINT('',(0.,32.,52.));
#5700=CARTESIAN_POINT('',(0.,0.,52.));
#5701=CARTESIAN_POINT('',(0.,32.,11.));
#5702=CARTESIAN_POINT('',(0.,32.,20.5));
#5703=CARTESIAN_POINT('',(-1.88109076926235E-16,34.9999999999997,5.80384757729367));
#5704=CARTESIAN_POINT('Origin',(0.,38.,11.));
#5705=CARTESIAN_POINT('',(0.,35.,0.));
#5706=CARTESIAN_POINT('',(0.,35.,0.));
#5707=CARTESIAN_POINT('',(0.,0.,0.));
#5708=CARTESIAN_POINT('Origin',(184.,0.,0.));
#5709=CARTESIAN_POINT('',(184.,-35.,0.));
#5710=CARTESIAN_POINT('',(184.,0.,0.));
#5711=CARTESIAN_POINT('',(128.131421846764,-37.7096774193548,0.));
#5712=CARTESIAN_POINT('Origin',(156.,-35.,0.));
#5713=CARTESIAN_POINT('',(125.145502758917,-35.,0.));
#5714=CARTESIAN_POINT('Origin',(125.145502758917,-38.,0.));
#5715=CARTESIAN_POINT('',(58.854497241083,-35.,0.));
#5716=CARTESIAN_POINT('',(0.,-35.,0.));
#5717=CARTESIAN_POINT('',(55.8685781532363,-37.7096774193548,0.));
#5718=CARTESIAN_POINT('Origin',(58.854497241083,-38.,0.));
#5719=CARTESIAN_POINT('Origin',(28.,-35.,0.));
#5720=CARTESIAN_POINT('',(24.,-50.,0.));
#5721=CARTESIAN_POINT('Origin',(28.,-50.,0.));
#5722=CARTESIAN_POINT('',(152.,-50.,0.));
#5723=CARTESIAN_POINT('Origin',(156.,-50.,0.));
#5724=CARTESIAN_POINT('Ctrl Pts',(3.,36.4999999999997,8.40192378864683));
#5725=CARTESIAN_POINT('Ctrl Pts',(2.99999999999998,36.954480338638,8.13952944279256));
#5726=CARTESIAN_POINT('Ctrl Pts',(3.05470342200826,37.4790034882233,8.));
#5727=CARTESIAN_POINT('Ctrl Pts',(3.18065270801829,38.,8.));
#5728=CARTESIAN_POINT('Ctrl Pts',(2.10240209897434,36.4999999999997,8.40192378864684));
#5729=CARTESIAN_POINT('Ctrl Pts',(2.11299837157538,36.9775281360311,8.12577095949316));
#5730=CARTESIAN_POINT('Ctrl Pts',(2.17111074773699,37.5492218178523,7.98077045544578));
#5731=CARTESIAN_POINT('Ctrl Pts',(2.28954094665391,38.1077117481231,8.));
#5732=CARTESIAN_POINT('Ctrl Pts',(0.547958039803657,36.1236422123021,7.75005297853055));
#5733=CARTESIAN_POINT('Ctrl Pts',(0.575502703260674,36.7685292312036,7.39913053299978));
#5734=CARTESIAN_POINT('Ctrl Pts',(0.639381985506942,37.5362747159179,7.21746293992274));
#5735=CARTESIAN_POINT('Ctrl Pts',(0.746329468633318,38.2942450352236,7.24728442460496));
#5736=CARTESIAN_POINT('Ctrl Pts',(-5.28707639943152E-15,35.3365992128841,
6.38685451579749));
#5737=CARTESIAN_POINT('Ctrl Pts',(0.0123332119636002,36.2492271656458,5.91410134300127));
#5738=CARTESIAN_POINT('Ctrl Pts',(0.0752933955656041,37.3077055625156,5.66439679042059));
#5739=CARTESIAN_POINT('Ctrl Pts',(0.202331032980483,38.36,5.67319842576924));
#5740=CARTESIAN_POINT('Ctrl Pts',(2.22044604925031E-15,34.9999999999994,
5.80384757729366));
#5741=CARTESIAN_POINT('Ctrl Pts',(-1.91613381295638E-14,36.0180359585492,
5.27905888558515));
#5742=CARTESIAN_POINT('Ctrl Pts',(0.0612678326492503,37.1929678136203,5.));
#5743=CARTESIAN_POINT('Ctrl Pts',(0.202331032980483,38.36,5.));
#5744=CARTESIAN_POINT('',(3.18065270801829,38.,8.));
#5745=CARTESIAN_POINT('',(0.202331032980484,38.36,5.));
#5746=CARTESIAN_POINT('Origin',(3.18065270801829,38.,5.));
#5747=CARTESIAN_POINT('Ctrl Pts',(0.202331032980483,38.36,5.));
#5748=CARTESIAN_POINT('Ctrl Pts',(0.0612678326492503,37.1929678136203,5.));
#5749=CARTESIAN_POINT('Ctrl Pts',(-1.91613381295638E-14,36.0180359585492,
5.27905888558515));
#5750=CARTESIAN_POINT('Ctrl Pts',(2.22044604925031E-15,34.9999999999994,
5.80384757729366));
#5751=CARTESIAN_POINT('',(3.,36.4999999999997,8.40192378864683));
#5752=CARTESIAN_POINT('Origin',(3.,34.9999999999995,5.80384757729367));
#5753=CARTESIAN_POINT('Ctrl Pts',(3.,36.4999999999997,8.40192378864683));
#5754=CARTESIAN_POINT('Ctrl Pts',(2.99999999999998,36.954480338638,8.13952944279256));
#5755=CARTESIAN_POINT('Ctrl Pts',(3.05470342200826,37.4790034882233,8.));
#5756=CARTESIAN_POINT('Ctrl Pts',(3.18065270801829,38.,8.));
#5757=CARTESIAN_POINT('Origin',(28.,35.,5.));
#5758=CARTESIAN_POINT('',(52.8193472919817,38.,8.));
#5759=CARTESIAN_POINT('',(55.7976689670195,38.36,5.));
#5760=CARTESIAN_POINT('Origin',(52.8193472919817,38.,5.));
#5761=CARTESIAN_POINT('Origin',(28.,35.,5.));
#5762=CARTESIAN_POINT('Origin',(28.,35.,8.));
#5763=CARTESIAN_POINT('Ctrl Pts',(55.8685781532363,37.7096774193548,5.02816182430651));
#5764=CARTESIAN_POINT('Ctrl Pts',(55.8475407647763,37.926043434088,5.00937844175291));
#5765=CARTESIAN_POINT('Ctrl Pts',(55.8238771966224,38.1431762825265,5.));
#5766=CARTESIAN_POINT('Ctrl Pts',(55.7976689670195,38.36,5.));
#5767=CARTESIAN_POINT('Ctrl Pts',(55.8602609046479,37.7952189272299,5.91625914580451));
#5768=CARTESIAN_POINT('Ctrl Pts',(55.8413719151341,37.9830850669533,5.90163360405696));
#5769=CARTESIAN_POINT('Ctrl Pts',(55.8203385684754,38.1717572674891,5.89534108170859));
#5770=CARTESIAN_POINT('Ctrl Pts',(55.7976689670195,38.36,5.89759790102565));
#5771=CARTESIAN_POINT('Ctrl Pts',(55.1056560895983,37.8713923378241,7.45429472319515));
#5772=CARTESIAN_POINT('Ctrl Pts',(55.0885194723629,38.0040411687438,7.44665978236163));
#5773=CARTESIAN_POINT('Ctrl Pts',(55.0699339818664,38.1370427186257,7.44582650050821));
#5774=CARTESIAN_POINT('Ctrl Pts',(55.0499325631178,38.2696185252047,7.45169302838196));
#5775=CARTESIAN_POINT('Ctrl Pts',(53.548732056513,37.7738335502611,8.00784297571193));
#5776=CARTESIAN_POINT('Ctrl Pts',(53.5304285848741,37.875964951252,8.00001814579437));
#5777=CARTESIAN_POINT('Ctrl Pts',(53.51008589056,37.978663056326,7.99737324321024));
#5778=CARTESIAN_POINT('Ctrl Pts',(53.487681113005,38.0807838110923,8.));
#5779=CARTESIAN_POINT('Ctrl Pts',(52.8826590653895,37.7096774193548,8.01408091215326));
#5780=CARTESIAN_POINT('Ctrl Pts',(52.8638756828359,37.8062693902182,8.00468922087643));
#5781=CARTESIAN_POINT('Ctrl Pts',(52.8427474969843,37.9032036975564,8.));
#5782=CARTESIAN_POINT('Ctrl Pts',(52.8193472919817,38.,8.));
#5783=CARTESIAN_POINT('',(52.8826590653895,37.7096774193548,8.01408091215326));
#5784=CARTESIAN_POINT('Ctrl Pts',(52.8193472919817,38.,8.));
#5785=CARTESIAN_POINT('Ctrl Pts',(52.8427474969843,37.9032036975564,8.));
#5786=CARTESIAN_POINT('Ctrl Pts',(52.8638756828359,37.8062693902182,8.00468922087643));
#5787=CARTESIAN_POINT('Ctrl Pts',(52.8826590653895,37.7096774193548,8.01408091215326));
#5788=CARTESIAN_POINT('',(55.8685781532363,37.7096774193548,5.02816182430651));
#5789=CARTESIAN_POINT('Origin',(52.8826590653895,37.4193548387097,5.02816182430651));
#5790=CARTESIAN_POINT('Ctrl Pts',(55.8685781532363,37.7096774193548,5.02816182430651));
#5791=CARTESIAN_POINT('Ctrl Pts',(55.8475407647763,37.926043434088,5.00937844175291));
#5792=CARTESIAN_POINT('Ctrl Pts',(55.8238771966224,38.1431762825265,5.));
#5793=CARTESIAN_POINT('Ctrl Pts',(55.7976689670195,38.36,5.));
#5794=CARTESIAN_POINT('Ctrl Pts',(52.8826590653895,37.7096774193548,8.01408091215326));
#5795=CARTESIAN_POINT('Ctrl Pts',(52.9234112434749,37.5001127583042,8.03445700119595));
#5796=CARTESIAN_POINT('Ctrl Pts',(53.1775159289433,36.8777334443635,8.16150934393013));
#5797=CARTESIAN_POINT('Ctrl Pts',(54.243086357739,35.9425957985175,8.69429455832799));
#5798=CARTESIAN_POINT('Ctrl Pts',(56.3283651995436,35.1800659070611,9.73693397923028));
#5799=CARTESIAN_POINT('Ctrl Pts',(58.0122855606517,35.,10.5788941597843));
#5800=CARTESIAN_POINT('Ctrl Pts',(58.854497241083,35.,11.));
#5801=CARTESIAN_POINT('Ctrl Pts',(53.7707563868875,37.7952189272299,8.00576366356483));
#5802=CARTESIAN_POINT('Ctrl Pts',(53.7976964911934,37.6462990978492,8.01387139589604));
#5803=CARTESIAN_POINT('Ctrl Pts',(53.9641832386802,37.1877421817658,8.06350064714943));
#5804=CARTESIAN_POINT('Ctrl Pts',(54.7636697148025,36.2427780971064,8.41333065085001));
#5805=CARTESIAN_POINT('Ctrl Pts',(56.5682125706966,35.2513707994457,9.49453429056375));
#5806=CARTESIAN_POINT('Ctrl Pts',(58.0924961968832,35.,10.4986835235528));
#5807=CARTESIAN_POINT('Ctrl Pts',(58.854497241083,35.,11.));
#5808=CARTESIAN_POINT('Ctrl Pts',(55.3087758987271,37.8713886997517,7.25113749710106));
#5809=CARTESIAN_POINT('Ctrl Pts',(55.3128774402037,37.7745857657828,7.25775185774585));
#5810=CARTESIAN_POINT('Ctrl Pts',(55.332435648546,37.4546465421952,7.29305669671663));
#5811=CARTESIAN_POINT('Ctrl Pts',(55.6785458516857,36.4828390697622,7.69460851516791));
#5812=CARTESIAN_POINT('Ctrl Pts',(56.9905659808484,35.3039288072282,9.07594546731005));
#5813=CARTESIAN_POINT('Ctrl Pts',(58.2328648102884,35.,10.3583149101475));
#5814=CARTESIAN_POINT('Ctrl Pts',(58.854497241083,35.,11.));
#5815=CARTESIAN_POINT('Ctrl Pts',(55.862340216795,37.7738335502611,5.69423481543001));
#5816=CARTESIAN_POINT('Ctrl Pts',(55.8737235797682,37.6091470033402,5.72485515984047));
#5817=CARTESIAN_POINT('Ctrl Pts',(55.9430708156095,37.1082524544471,5.91363113676918));
#5818=CARTESIAN_POINT('Ctrl Pts',(56.339900292733,36.1672073699739,6.78103264850998));
#5819=CARTESIAN_POINT('Ctrl Pts',(57.4107265395028,35.2340992431039,8.6549624533521));
#5820=CARTESIAN_POINT('Ctrl Pts',(58.3732334236937,35.,10.2179462967423));
#5821=CARTESIAN_POINT('Ctrl Pts',(58.854497241083,35.,11.));
#5822=CARTESIAN_POINT('Ctrl Pts',(55.8685781532363,37.7096774193548,5.02816182430651));
#5823=CARTESIAN_POINT('Ctrl Pts',(55.888954242279,37.5001127583042,5.0689140023919));
#5824=CARTESIAN_POINT('Ctrl Pts',(56.0160065850132,36.8777334443635,5.32301868786026));
#5825=CARTESIAN_POINT('Ctrl Pts',(56.548791799411,35.9425957985175,6.38858911665598));
#5826=CARTESIAN_POINT('Ctrl Pts',(57.5914312203133,35.1800659070611,8.47386795846057));
#5827=CARTESIAN_POINT('Ctrl Pts',(58.4333914008674,35.,10.1577883195686));
#5828=CARTESIAN_POINT('Ctrl Pts',(58.854497241083,35.,11.));
#5829=CARTESIAN_POINT('',(58.854497241083,35.,11.));
#5830=CARTESIAN_POINT('Origin',(58.854497241083,38.,11.));
#5831=CARTESIAN_POINT('Origin',(58.854497241083,38.,11.));
#5832=CARTESIAN_POINT('Origin',(35.,32.,52.));
#5833=CARTESIAN_POINT('',(16.97224362268,32.,82.));
#5834=CARTESIAN_POINT('',(23.8644712743399,35.,82.));
#5835=CARTESIAN_POINT('Ctrl Pts',(16.97224362268,32.,82.));
#5836=CARTESIAN_POINT('Ctrl Pts',(16.97224362268,32.1342826532508,82.));
#5837=CARTESIAN_POINT('Ctrl Pts',(16.9946832528106,32.2938517592452,82.));
#5838=CARTESIAN_POINT('Ctrl Pts',(17.0702539988253,32.5663418025556,82.));
#5839=CARTESIAN_POINT('Ctrl Pts',(17.1416262957653,32.7296146052374,82.));
#5840=CARTESIAN_POINT('Ctrl Pts',(17.4226441511211,33.2098600173186,82.));
#5841=CARTESIAN_POINT('Ctrl Pts',(17.7820383793495,33.5422189915824,82.));
#5842=CARTESIAN_POINT('Ctrl Pts',(18.6622714155113,34.1331069213694,82.));
#5843=CARTESIAN_POINT('Ctrl Pts',(19.3931201505777,34.413210266344,82.));
#5844=CARTESIAN_POINT('Ctrl Pts',(20.6104592865239,34.7357198507857,82.));
#5845=CARTESIAN_POINT('Ctrl Pts',(21.2666393342951,34.845555358661,82.));
#5846=CARTESIAN_POINT('Ctrl Pts',(22.5901610524715,34.9770485861857,82.));
#5847=CARTESIAN_POINT('Ctrl Pts',(23.2573738737762,35.,82.));
#5848=CARTESIAN_POINT('Ctrl Pts',(23.8644712743399,35.,82.));
#5849=CARTESIAN_POINT('',(3.,35.,52.));
#5850=CARTESIAN_POINT('Origin',(35.,35.,52.));
#5851=CARTESIAN_POINT('Origin',(3.,32.,52.));
#5852=CARTESIAN_POINT('Origin',(35.,32.,52.));
#5853=CARTESIAN_POINT('Origin',(3.,32.,20.5));
#5854=CARTESIAN_POINT('',(3.,35.,11.));
#5855=CARTESIAN_POINT('Origin',(3.,32.,11.));
#5856=CARTESIAN_POINT('',(3.,35.,20.5));
#5857=CARTESIAN_POINT('Origin',(3.,38.,11.));
#5858=CARTESIAN_POINT('Origin',(3.,38.,11.));
#5859=CARTESIAN_POINT('Origin',(58.854497241083,38.,0.));
#5860=CARTESIAN_POINT('',(58.854497241083,35.,0.));
#5861=CARTESIAN_POINT('',(58.854497241083,35.,0.));
#5862=CARTESIAN_POINT('',(55.8685781532363,37.7096774193548,0.));
#5863=CARTESIAN_POINT('Origin',(58.854497241083,38.,0.));
#5864=CARTESIAN_POINT('',(55.8685781532363,37.7096774193548,0.));
#5865=CARTESIAN_POINT('Origin',(28.,49.,8.));
#5866=CARTESIAN_POINT('',(60.,38.,8.));
#5867=CARTESIAN_POINT('',(24.,50.,8.));
#5868=CARTESIAN_POINT('Origin',(28.,50.,8.));
#5869=CARTESIAN_POINT('Origin',(60.,38.,11.));
#5870=CARTESIAN_POINT('',(60.,35.,11.));
#5871=CARTESIAN_POINT('Origin',(92.,35.,41.));
#5872=CARTESIAN_POINT('',(31.47224362268,35.,82.));
#5873=CARTESIAN_POINT('',(158.47224362268,35.,52.7659032476128));
#5874=CARTESIAN_POINT('',(158.47224362268,35.,74.9975567301459));
#5875=CARTESIAN_POINT('',(180.509407751081,35.,52.9699515362416));
#5876=CARTESIAN_POINT('',(137.703021578879,35.,52.5735951906642));
#5877=CARTESIAN_POINT('',(180.898019313572,35.,11.));
#5878=CARTESIAN_POINT('',(180.542507983541,35.,49.3951347106504));
#5879=CARTESIAN_POINT('',(125.145502758917,35.,11.));
#5880=CARTESIAN_POINT('',(124.,35.,11.));
#5881=CARTESIAN_POINT('',(125.145502758917,35.,0.));
#5882=CARTESIAN_POINT('',(125.145502758917,35.,0.));
#5883=CARTESIAN_POINT('',(0.,35.,0.));
#5884=CARTESIAN_POINT('Origin',(35.,-32.,52.));
#5885=CARTESIAN_POINT('',(23.8644712743399,-35.,82.));
#5886=CARTESIAN_POINT('',(16.97224362268,-32.,82.));
#5887=CARTESIAN_POINT('Ctrl Pts',(23.8644712743399,-35.,82.));
#5888=CARTESIAN_POINT('Ctrl Pts',(23.2573738737762,-35.,82.));
#5889=CARTESIAN_POINT('Ctrl Pts',(22.5901610524715,-34.9770485861857,82.));
#5890=CARTESIAN_POINT('Ctrl Pts',(21.2666393342951,-34.845555358661,82.));
#5891=CARTESIAN_POINT('Ctrl Pts',(20.6104592865239,-34.7357198507857,82.));
#5892=CARTESIAN_POINT('Ctrl Pts',(19.3931201505777,-34.413210266344,82.));
#5893=CARTESIAN_POINT('Ctrl Pts',(18.6622714155113,-34.1331069213694,82.));
#5894=CARTESIAN_POINT('Ctrl Pts',(17.7820383793495,-33.5422189915824,82.));
#5895=CARTESIAN_POINT('Ctrl Pts',(17.4226441511211,-33.2098600173186,82.));
#5896=CARTESIAN_POINT('Ctrl Pts',(17.1416262957653,-32.7296146052374,82.));
#5897=CARTESIAN_POINT('Ctrl Pts',(17.0702539988253,-32.5663418025556,82.));
#5898=CARTESIAN_POINT('Ctrl Pts',(16.9946832528106,-32.2938517592452,82.));
#5899=CARTESIAN_POINT('Ctrl Pts',(16.97224362268,-32.1342826532508,82.));
#5900=CARTESIAN_POINT('Ctrl Pts',(16.97224362268,-32.,82.));
#5901=CARTESIAN_POINT('Origin',(35.,-32.,52.));
#5902=CARTESIAN_POINT('',(3.,-35.,52.));
#5903=CARTESIAN_POINT('Origin',(3.,-32.,52.));
#5904=CARTESIAN_POINT('Origin',(35.,-35.,52.));
#5905=CARTESIAN_POINT('Origin',(3.,-32.,20.5));
#5906=CARTESIAN_POINT('',(3.,-35.,11.));
#5907=CARTESIAN_POINT('Origin',(3.,-32.,11.));
#5908=CARTESIAN_POINT('',(3.,-35.,20.5));
#5909=CARTESIAN_POINT('Ctrl Pts',(5.55111512312578E-16,-34.9999999999998,
5.80384757729347));
#5910=CARTESIAN_POINT('Ctrl Pts',(-6.79692625904774E-15,-36.0180282120301,
5.27906287884847));
#5911=CARTESIAN_POINT('Ctrl Pts',(0.0612689060384735,-37.1929766938936,
5.));
#5912=CARTESIAN_POINT('Ctrl Pts',(0.20233103298048,-38.36,5.));
#5913=CARTESIAN_POINT('Ctrl Pts',(-2.7666680096006E-15,-35.4487989505127,
6.58119016196527));
#5914=CARTESIAN_POINT('Ctrl Pts',(0.016774360715285,-36.3253230330411,6.12605195674292));
#5915=CARTESIAN_POINT('Ctrl Pts',(0.0803150766662462,-37.3468098443969,
5.88545088698412));
#5916=CARTESIAN_POINT('Ctrl Pts',(0.20233103298048,-38.36,5.89759790102566));
#5917=CARTESIAN_POINT('Ctrl Pts',(0.752715575395041,-36.226020980098,7.92737820596885));
#5918=CARTESIAN_POINT('Ctrl Pts',(0.778729521784382,-36.8315954742153,7.59307849185768));
#5919=CARTESIAN_POINT('Ctrl Pts',(0.841952567680975,-37.5561034113538,7.42046619517227));
#5920=CARTESIAN_POINT('Ctrl Pts',(0.94960740409302,-38.2696741309526,7.45204196019633));
#5921=CARTESIAN_POINT('Ctrl Pts',(2.32680157423076,-36.4999999999999,8.40192378864674));
#5922=CARTESIAN_POINT('Ctrl Pts',(2.33447943710505,-36.9723882847684,8.12903347048555));
#5923=CARTESIAN_POINT('Ctrl Pts',(2.39172830825428,-37.5311331444668,7.98586184929931));
#5924=CARTESIAN_POINT('Ctrl Pts',(2.512318886995,-38.0807838110923,8.));
#5925=CARTESIAN_POINT('Ctrl Pts',(3.,-36.4999999999999,8.40192378864674));
#5926=CARTESIAN_POINT('Ctrl Pts',(2.99999999999999,-36.9544768803712,8.13953143942391));
#5927=CARTESIAN_POINT('Ctrl Pts',(3.05470438039141,-37.4790074526303,8.));
#5928=CARTESIAN_POINT('Ctrl Pts',(3.18065270801828,-38.,8.));
#5929=CARTESIAN_POINT('',(0.20233103298048,-38.36,5.));
#5930=CARTESIAN_POINT('',(3.18065270801828,-38.,8.));
#5931=CARTESIAN_POINT('Origin',(3.18065270801829,-38.,5.));
#5932=CARTESIAN_POINT('',(3.,-36.4999999999999,8.40192378864674));
#5933=CARTESIAN_POINT('Ctrl Pts',(3.18065270801828,-38.,8.));
#5934=CARTESIAN_POINT('Ctrl Pts',(3.05470438039141,-37.4790074526303,8.));
#5935=CARTESIAN_POINT('Ctrl Pts',(2.99999999999999,-36.9544768803712,8.13953143942391));
#5936=CARTESIAN_POINT('Ctrl Pts',(3.,-36.4999999999999,8.40192378864674));
#5937=CARTESIAN_POINT('Origin',(3.,-34.9999999999998,5.80384757729347));
#5938=CARTESIAN_POINT('Ctrl Pts',(5.55111512312578E-16,-34.9999999999998,
5.80384757729347));
#5939=CARTESIAN_POINT('Ctrl Pts',(-6.79692625904774E-15,-36.0180282120301,
5.27906287884847));
#5940=CARTESIAN_POINT('Ctrl Pts',(0.0612689060384735,-37.1929766938936,
5.));
#5941=CARTESIAN_POINT('Ctrl Pts',(0.20233103298048,-38.36,5.));
#5942=CARTESIAN_POINT('Origin',(28.,-35.,5.));
#5943=CARTESIAN_POINT('',(55.7976689670195,-38.36,5.));
#5944=CARTESIAN_POINT('',(52.8193472919817,-38.,8.));
#5945=CARTESIAN_POINT('Origin',(52.8193472919817,-38.,5.));
#5946=CARTESIAN_POINT('Origin',(28.,-35.,8.));
#5947=CARTESIAN_POINT('Origin',(28.,-35.,5.));
#5948=CARTESIAN_POINT('Ctrl Pts',(55.7976689670195,-38.36,5.));
#5949=CARTESIAN_POINT('Ctrl Pts',(55.8238771966224,-38.1431762825264,5.));
#5950=CARTESIAN_POINT('Ctrl Pts',(55.8475407647763,-37.926043434088,5.00937844175291));
#5951=CARTESIAN_POINT('Ctrl Pts',(55.8685781532363,-37.7096774193548,5.02816182430651));
#5952=CARTESIAN_POINT('Ctrl Pts',(55.7976689670195,-38.36,5.89759790102566));
#5953=CARTESIAN_POINT('Ctrl Pts',(55.8203385684754,-38.1717572674891,5.89534108170859));
#5954=CARTESIAN_POINT('Ctrl Pts',(55.8413719151341,-37.9830850669531,5.90163360405697));
#5955=CARTESIAN_POINT('Ctrl Pts',(55.8602609046479,-37.7952189272299,5.91625914580451));
#5956=CARTESIAN_POINT('Ctrl Pts',(55.0499325631178,-38.2696185252047,7.45169302838196));
#5957=CARTESIAN_POINT('Ctrl Pts',(55.0699339818664,-38.1370427186258,7.44582650050821));
#5958=CARTESIAN_POINT('Ctrl Pts',(55.0885194723629,-38.0040411687434,7.44665978236167));
#5959=CARTESIAN_POINT('Ctrl Pts',(55.1056560895983,-37.8713923378241,7.45429472319515));
#5960=CARTESIAN_POINT('Ctrl Pts',(53.487681113005,-38.0807838110923,8.));
#5961=CARTESIAN_POINT('Ctrl Pts',(53.51008589056,-37.9786630563262,7.99737324321024));
#5962=CARTESIAN_POINT('Ctrl Pts',(53.5304285848741,-37.8759649512515,8.00001814579442));
#5963=CARTESIAN_POINT('Ctrl Pts',(53.548732056513,-37.7738335502611,8.00784297571193));
#5964=CARTESIAN_POINT('Ctrl Pts',(52.8193472919817,-38.,8.));
#5965=CARTESIAN_POINT('Ctrl Pts',(52.8427474969842,-37.9032036975566,8.));
#5966=CARTESIAN_POINT('Ctrl Pts',(52.863875682836,-37.8062693902177,8.00468922087647));
#5967=CARTESIAN_POINT('Ctrl Pts',(52.8826590653895,-37.7096774193548,8.01408091215325));
#5968=CARTESIAN_POINT('',(55.8685781532363,-37.7096774193548,5.02816182430651));
#5969=CARTESIAN_POINT('',(52.8826590653895,-37.7096774193548,8.01408091215326));
#5970=CARTESIAN_POINT('Origin',(52.8826590653895,-37.4193548387097,5.02816182430651));
#5971=CARTESIAN_POINT('Ctrl Pts',(52.8826590653895,-37.7096774193548,8.01408091215325));
#5972=CARTESIAN_POINT('Ctrl Pts',(52.863875682836,-37.8062693902177,8.00468922087647));
#5973=CARTESIAN_POINT('Ctrl Pts',(52.8427474969842,-37.9032036975566,8.));
#5974=CARTESIAN_POINT('Ctrl Pts',(52.8193472919817,-38.,8.));
#5975=CARTESIAN_POINT('Ctrl Pts',(55.7976689670195,-38.36,5.));
#5976=CARTESIAN_POINT('Ctrl Pts',(55.8238771966224,-38.1431762825264,5.));
#5977=CARTESIAN_POINT('Ctrl Pts',(55.8475407647763,-37.926043434088,5.00937844175291));
#5978=CARTESIAN_POINT('Ctrl Pts',(55.8685781532363,-37.7096774193548,5.02816182430651));
#5979=CARTESIAN_POINT('Ctrl Pts',(58.854497241083,-35.,11.));
#5980=CARTESIAN_POINT('Ctrl Pts',(57.591179720436,-35.,10.3683412396765));
#5981=CARTESIAN_POINT('Ctrl Pts',(55.491665523271,-35.3447900318788,9.31858414109399));
#5982=CARTESIAN_POINT('Ctrl Pts',(53.4860813463977,-36.4709655486432,8.31579205265733));
#5983=CARTESIAN_POINT('Ctrl Pts',(52.9641634215603,-37.2905480972536,8.05483309023865));
#5984=CARTESIAN_POINT('Ctrl Pts',(52.8826590653895,-37.7096774193548,8.01408091215326));
#5985=CARTESIAN_POINT('Ctrl Pts',(58.854497241083,-35.,11.));
#5986=CARTESIAN_POINT('Ctrl Pts',(57.7114956747833,-35.,10.2480252853291));
#5987=CARTESIAN_POINT('Ctrl Pts',(55.8108578482975,-35.49734135073,9.00048604592416));
#5988=CARTESIAN_POINT('Ctrl Pts',(54.1695839772935,-36.8310361085116,8.12526335720806));
#5989=CARTESIAN_POINT('Ctrl Pts',(53.8246365954992,-37.4973792684685,8.02197912822726));
#5990=CARTESIAN_POINT('Ctrl Pts',(53.7707563868875,-37.7952189272299,8.00576366356483));
#5991=CARTESIAN_POINT('Ctrl Pts',(58.854497241083,-35.,11.));
#5992=CARTESIAN_POINT('Ctrl Pts',(57.9220485948912,-35.,10.0374723652213));
#5993=CARTESIAN_POINT('Ctrl Pts',(56.3761160372177,-35.6097541353715,8.44025943776391));
#5994=CARTESIAN_POINT('Ctrl Pts',(55.3639766415692,-37.1311590010604,7.3440863877359));
#5995=CARTESIAN_POINT('Ctrl Pts',(55.3169789816803,-37.677782831814,7.26436621839063));
#5996=CARTESIAN_POINT('Ctrl Pts',(55.3087758987271,-37.8713886997517,7.25113749710106));
#5997=CARTESIAN_POINT('Ctrl Pts',(58.854497241083,-35.,11.));
#5998=CARTESIAN_POINT('Ctrl Pts',(58.132601514999,-35.,9.82691944511346));
#5999=CARTESIAN_POINT('Ctrl Pts',(56.9368441486366,-35.4601371544742,7.87913897720146));
#6000=CARTESIAN_POINT('Ctrl Pts',(56.0284907858974,-36.7392653296661,6.14540023341453));
#6001=CARTESIAN_POINT('Ctrl Pts',(55.8851069427414,-37.4444604564192,5.75547550425093));
#6002=CARTESIAN_POINT('Ctrl Pts',(55.862340216795,-37.7738335502611,5.69423481543001));
#6003=CARTESIAN_POINT('Ctrl Pts',(58.854497241083,-35.,11.));
#6004=CARTESIAN_POINT('Ctrl Pts',(58.2228384807595,-35.,9.73668247935295));
#6005=CARTESIAN_POINT('Ctrl Pts',(57.173081382177,-35.3447900318788,7.63716828218798));
#6006=CARTESIAN_POINT('Ctrl Pts',(56.1702892937404,-36.4709655486432,5.63158410531467));
#6007=CARTESIAN_POINT('Ctrl Pts',(55.9093303313217,-37.2905480972536,5.10966618047728));
#6008=CARTESIAN_POINT('Ctrl Pts',(55.8685781532363,-37.7096774193548,5.02816182430651));
#6009=CARTESIAN_POINT('',(58.854497241083,-35.,11.));
#6010=CARTESIAN_POINT('Origin',(58.854497241083,-38.,11.));
#6011=CARTESIAN_POINT('Origin',(58.854497241083,-38.,11.));
#6012=CARTESIAN_POINT('Origin',(3.,-38.,11.));
#6013=CARTESIAN_POINT('Origin',(3.,-38.,11.));
#6014=CARTESIAN_POINT('Origin',(28.,-49.,8.));
#6015=CARTESIAN_POINT('',(60.,-38.,8.));
#6016=CARTESIAN_POINT('',(24.,-50.,8.));
#6017=CARTESIAN_POINT('Origin',(28.,-50.,8.));
#6018=CARTESIAN_POINT('Origin',(58.854497241083,-38.,0.));
#6019=CARTESIAN_POINT('',(55.8685781532363,-37.7096774193548,0.));
#6020=CARTESIAN_POINT('',(58.854497241083,-35.,0.));
#6021=CARTESIAN_POINT('Origin',(28.,-35.,0.));
#6022=CARTESIAN_POINT('Ctrl Pts',(125.145502758917,35.,11.));
#6023=CARTESIAN_POINT('Ctrl Pts',(126.408820279564,35.,10.3683412396765));
#6024=CARTESIAN_POINT('Ctrl Pts',(128.508262002194,35.3448821043614,9.31862037836163));
#6025=CARTESIAN_POINT('Ctrl Pts',(130.513866046969,36.4710105181724,8.31581835597387));
#6026=CARTESIAN_POINT('Ctrl Pts',(131.03583657844,37.2905480972536,8.05483309023865));
#6027=CARTESIAN_POINT('Ctrl Pts',(131.11734093461,37.7096774193548,8.01408091215326));
#6028=CARTESIAN_POINT('Ctrl Pts',(125.145502758917,35.,11.));
#6029=CARTESIAN_POINT('Ctrl Pts',(126.288504325217,35.,10.2480252853291));
#6030=CARTESIAN_POINT('Ctrl Pts',(128.189273783442,35.4974603268054,9.00013278294707));
#6031=CARTESIAN_POINT('Ctrl Pts',(129.830512389917,36.8310532862727,8.12500325624924));
#6032=CARTESIAN_POINT('Ctrl Pts',(130.175363404501,37.4973792684685,8.02197912822726));
#6033=CARTESIAN_POINT('Ctrl Pts',(130.229243613112,37.7952189272299,8.00576366356483));
#6034=CARTESIAN_POINT('Ctrl Pts',(125.145502758917,35.,11.));
#6035=CARTESIAN_POINT('Ctrl Pts',(126.077951405109,35.,10.0374723652213));
#6036=CARTESIAN_POINT('Ctrl Pts',(127.623980299275,35.6097041403199,8.44014872177682));
#6037=CARTESIAN_POINT('Ctrl Pts',(128.636157969133,37.1308061894763,7.34393528770233));
#6038=CARTESIAN_POINT('Ctrl Pts',(128.683173815107,37.6777482307114,7.26416314863648));
#6039=CARTESIAN_POINT('Ctrl Pts',(128.69137689806,37.8713540986491,7.25093442734691));
#6040=CARTESIAN_POINT('Ctrl Pts',(125.145502758917,35.,11.));
#6041=CARTESIAN_POINT('Ctrl Pts',(125.867398485001,35.,9.82691944511346));
#6042=CARTESIAN_POINT('Ctrl Pts',(127.063224468555,35.4602324624254,7.87926400736172));
#6043=CARTESIAN_POINT('Ctrl Pts',(127.971574547182,36.7392080834518,6.14547579678636));
#6044=CARTESIAN_POINT('Ctrl Pts',(128.114893057259,37.4444604564192,5.75547550425093));
#6045=CARTESIAN_POINT('Ctrl Pts',(128.137659783205,37.7738335502611,5.69423481543001));
#6046=CARTESIAN_POINT('Ctrl Pts',(125.145502758917,35.,11.));
#6047=CARTESIAN_POINT('Ctrl Pts',(125.777161519241,35.,9.73668247935295));
#6048=CARTESIAN_POINT('Ctrl Pts',(126.826882380555,35.3448821043614,7.63724075672326));
#6049=CARTESIAN_POINT('Ctrl Pts',(127.829684402943,36.4710105181724,5.63163671194773));
#6050=CARTESIAN_POINT('Ctrl Pts',(128.090669668678,37.2905480972536,5.10966618047728));
#6051=CARTESIAN_POINT('Ctrl Pts',(128.131421846764,37.7096774193548,5.02816182430651));
#6052=CARTESIAN_POINT('',(131.11734093461,37.7096774193548,8.01408091215326));
#6053=CARTESIAN_POINT('',(128.131421846764,37.7096774193548,5.02816182430653));
#6054=CARTESIAN_POINT('Origin',(131.11734093461,37.4193548387097,5.02816182430651));
#6055=CARTESIAN_POINT('Origin',(125.145502758917,38.,11.));
#6056=CARTESIAN_POINT('Origin',(125.145502758917,38.,11.));
#6057=CARTESIAN_POINT('Ctrl Pts',(128.20233103298,38.36,5.));
#6058=CARTESIAN_POINT('Ctrl Pts',(128.176122803378,38.1431762825264,5.));
#6059=CARTESIAN_POINT('Ctrl Pts',(128.152459235224,37.926043434088,5.00937844175291));
#6060=CARTESIAN_POINT('Ctrl Pts',(128.131421846764,37.7096774193548,5.02816182430651));
#6061=CARTESIAN_POINT('Ctrl Pts',(128.20233103298,38.36,5.89759790102566));
#6062=CARTESIAN_POINT('Ctrl Pts',(128.179661431525,38.1717572674891,5.89534108170859));
#6063=CARTESIAN_POINT('Ctrl Pts',(128.158628084866,37.9830850669535,5.90163360405693));
#6064=CARTESIAN_POINT('Ctrl Pts',(128.139739095352,37.7952189272299,5.91625914580451));
#6065=CARTESIAN_POINT('Ctrl Pts',(128.950298064189,38.2695906484878,7.45151809910225));
#6066=CARTESIAN_POINT('Ctrl Pts',(128.93029664544,38.137014841909,7.4456515712285));
#6067=CARTESIAN_POINT('Ctrl Pts',(128.91170554589,38.0040028278322,7.44649047075606));
#6068=CARTESIAN_POINT('Ctrl Pts',(128.894568928654,37.8713539969117,7.45412541158964));
#6069=CARTESIAN_POINT('Ctrl Pts',(130.512318886995,38.0807838110923,8.00000000000001));
#6070=CARTESIAN_POINT('Ctrl Pts',(130.48991410944,37.9786630563264,7.99737324321024));
#6071=CARTESIAN_POINT('Ctrl Pts',(130.469571415126,37.8759649512528,8.00001814579429));
#6072=CARTESIAN_POINT('Ctrl Pts',(130.451267943487,37.7738335502611,8.00784297571193));
#6073=CARTESIAN_POINT('Ctrl Pts',(131.180652708018,38.,8.00000000000001));
#6074=CARTESIAN_POINT('Ctrl Pts',(131.157252503016,37.9032036975568,8.00000000000001));
#6075=CARTESIAN_POINT('Ctrl Pts',(131.136124317164,37.806269390219,8.00468922087635));
#6076=CARTESIAN_POINT('Ctrl Pts',(131.11734093461,37.7096774193548,8.01408091215326));
#6077=CARTESIAN_POINT('',(131.180652708018,38.,8.));
#6078=CARTESIAN_POINT('Ctrl Pts',(131.11734093461,37.7096774193548,8.01408091215326));
#6079=CARTESIAN_POINT('Ctrl Pts',(131.136124317164,37.806269390219,8.00468922087635));
#6080=CARTESIAN_POINT('Ctrl Pts',(131.157252503016,37.9032036975568,8.00000000000001));
#6081=CARTESIAN_POINT('Ctrl Pts',(131.180652708018,38.,8.00000000000001));
#6082=CARTESIAN_POINT('',(128.20233103298,38.36,5.));
#6083=CARTESIAN_POINT('Origin',(131.180652708018,38.,5.));
#6084=CARTESIAN_POINT('Ctrl Pts',(128.20233103298,38.36,5.));
#6085=CARTESIAN_POINT('Ctrl Pts',(128.176122803378,38.1431762825264,5.));
#6086=CARTESIAN_POINT('Ctrl Pts',(128.152459235224,37.926043434088,5.00937844175291));
#6087=CARTESIAN_POINT('Ctrl Pts',(128.131421846764,37.7096774193548,5.02816182430651));
#6088=CARTESIAN_POINT('Origin',(156.,35.,5.));
#6089=CARTESIAN_POINT('',(180.819347291982,38.,8.));
#6090=CARTESIAN_POINT('',(183.79766896702,38.36,5.));
#6091=CARTESIAN_POINT('Origin',(180.819347291982,38.,5.));
#6092=CARTESIAN_POINT('Origin',(156.,35.,5.));
#6093=CARTESIAN_POINT('Origin',(156.,35.,8.));
#6094=CARTESIAN_POINT('Ctrl Pts',(183.969815620835,33.7002253516408,6.67679159415515));
#6095=CARTESIAN_POINT('Ctrl Pts',(183.994326048599,34.2276645859955,6.2235861382656));
#6096=CARTESIAN_POINT('Ctrl Pts',(184.02615428097,35.6677168210592,5.33752658855133));
#6097=CARTESIAN_POINT('Ctrl Pts',(183.914814816133,37.390838829013,5.));
#6098=CARTESIAN_POINT('Ctrl Pts',(183.79766896702,38.36,5.));
#6099=CARTESIAN_POINT('Ctrl Pts',(183.999283936978,34.3343532523772,7.33713979338968));
#6100=CARTESIAN_POINT('Ctrl Pts',(184.007758579302,34.7839174007239,6.94606885961919));
#6101=CARTESIAN_POINT('Ctrl Pts',(184.00754893802,36.0206255096479,6.17500497055533));
#6102=CARTESIAN_POINT('Ctrl Pts',(183.898997814937,37.5185904475954,5.88751034382702));
#6103=CARTESIAN_POINT('Ctrl Pts',(183.79766896702,38.36,5.89759790102566));
#6104=CARTESIAN_POINT('Ctrl Pts',(183.264452217124,35.4676246877956,8.47924395641892));
#6105=CARTESIAN_POINT('Ctrl Pts',(183.263208393294,35.7681924393132,8.19574897233831));
#6106=CARTESIAN_POINT('Ctrl Pts',(183.243967632483,36.6145825085804,7.62528081991518));
#6107=CARTESIAN_POINT('Ctrl Pts',(183.139031868617,37.6769929878661,7.42524072691035));
#6108=CARTESIAN_POINT('Ctrl Pts',(183.049629294758,38.2695818681135,7.451463001346));
#6109=CARTESIAN_POINT('Ctrl Pts',(181.659660906753,35.90317816407,8.8543376916631));
#6110=CARTESIAN_POINT('Ctrl Pts',(181.674727762002,36.1417795639035,8.62106214617757));
#6111=CARTESIAN_POINT('Ctrl Pts',(181.689017399754,36.8060222478378,8.15740575482789));
#6112=CARTESIAN_POINT('Ctrl Pts',(181.587826247974,37.6243232752034,7.98825889198873));
#6113=CARTESIAN_POINT('Ctrl Pts',(181.487681113005,38.0807838110923,8.00000000000001));
#6114=CARTESIAN_POINT('Ctrl Pts',(180.973049661459,35.9197434605539,8.83839579707757));
#6115=CARTESIAN_POINT('Ctrl Pts',(180.994933971964,36.1552074044623,8.6117930691328));
#6116=CARTESIAN_POINT('Ctrl Pts',(181.023352036581,36.7980878665444,8.16876329427566));
#6117=CARTESIAN_POINT('Ctrl Pts',(180.923941800119,37.567338762952,8.00000000000001));
#6118=CARTESIAN_POINT('Ctrl Pts',(180.819347291982,38.,8.00000000000001));
#6119=CARTESIAN_POINT('',(183.402520572671,35.,8.));
#6120=CARTESIAN_POINT('',(184.,35.0000000000057,5.80384757728751));
#6121=CARTESIAN_POINT('Ctrl Pts',(183.402520572671,35.,8.00000000000001));
#6122=CARTESIAN_POINT('Ctrl Pts',(183.547773995999,35.,7.7333080978234));
#6123=CARTESIAN_POINT('Ctrl Pts',(183.671610877184,35.,7.45631037055478));
#6124=CARTESIAN_POINT('Ctrl Pts',(183.917381012336,35.,6.72638475914925));
#6125=CARTESIAN_POINT('Ctrl Pts',(184.,35.,6.2679088960418));
#6126=CARTESIAN_POINT('Ctrl Pts',(184.,35.,5.80384757729336));
#6127=CARTESIAN_POINT('Ctrl Pts',(184.000120745918,35.000102047304,5.80404540408506));
#6128=CARTESIAN_POINT('Ctrl Pts',(184.000133528268,35.1673874095417,5.71774484775865));
#6129=CARTESIAN_POINT('Ctrl Pts',(183.99092210883,36.2129801855919,5.23071994198585));
#6130=CARTESIAN_POINT('Ctrl Pts',(183.914814816133,37.390838829013,5.));
#6131=CARTESIAN_POINT('Ctrl Pts',(183.79766896702,38.36,5.));
#6132=CARTESIAN_POINT('',(180.951927409851,37.2748094254573,8.0889694899422));
#6133=CARTESIAN_POINT('Ctrl Pts',(180.819347291982,38.,8.00000000000001));
#6134=CARTESIAN_POINT('Ctrl Pts',(180.877934687157,37.7576498487013,8.00000000000001));
#6135=CARTESIAN_POINT('Ctrl Pts',(180.921528153108,37.5131314297474,8.03025732712463));
#6136=CARTESIAN_POINT('Ctrl Pts',(180.951190744332,37.2749112313906,8.08956288864171));
#6137=CARTESIAN_POINT('',(181.667890676754,37.2737119676904,8.));
#6138=CARTESIAN_POINT('Ctrl Pts',(180.951927410773,37.2748094100323,8.08896949376647));
#6139=CARTESIAN_POINT('Ctrl Pts',(180.956018127086,37.274924346416,8.088940861025));
#6140=CARTESIAN_POINT('Ctrl Pts',(180.960108840395,37.2750372329885,8.08890412577989));
#6141=CARTESIAN_POINT('Ctrl Pts',(181.201858997869,37.2815874148225,8.08625432298268));
#6142=CARTESIAN_POINT('Ctrl Pts',(181.438060925305,37.2810667321981,8.05631843825027));
#6143=CARTESIAN_POINT('Ctrl Pts',(181.667890676754,37.2737119676901,8.00000000000007));
#6144=CARTESIAN_POINT('Ctrl Pts',(181.667890676754,37.2737119676904,8.));
#6145=CARTESIAN_POINT('Ctrl Pts',(181.971820880737,36.9900034700373,8.));
#6146=CARTESIAN_POINT('Ctrl Pts',(182.272427380856,36.6776626323208,7.99999999958518));
#6147=CARTESIAN_POINT('Ctrl Pts',(182.944484312768,35.8457345941287,7.99999999958518));
#6148=CARTESIAN_POINT('Ctrl Pts',(183.212875666898,35.3970112792475,8.));
#6149=CARTESIAN_POINT('Ctrl Pts',(183.402520572671,35.,8.));
#6150=CARTESIAN_POINT('Origin',(156.,35.,0.));
#6151=CARTESIAN_POINT('',(184.,35.,0.));
#6152=CARTESIAN_POINT('',(184.,35.,0.));
#6153=CARTESIAN_POINT('',(128.131421846764,37.7096774193548,0.));
#6154=CARTESIAN_POINT('Origin',(156.,35.,0.));
#6155=CARTESIAN_POINT('',(128.131421846764,37.7096774193548,0.));
#6156=CARTESIAN_POINT('Origin',(128.,35.,0.));
#6157=CARTESIAN_POINT('',(183.368772894521,35.,7.99999999999765));
#6158=CARTESIAN_POINT('',(142.,35.,8.));
#6159=CARTESIAN_POINT('',(183.946003354294,35.,5.83162422873126));
#6160=CARTESIAN_POINT('Ctrl Pts',(183.36877289452,35.,7.99999999999716));
#6161=CARTESIAN_POINT('Ctrl Pts',(183.466406037598,35.,7.81137594025211));
#6162=CARTESIAN_POINT('Ctrl Pts',(183.555890991522,35.,7.61467203113216));
#6163=CARTESIAN_POINT('Ctrl Pts',(183.851877965836,35.,6.8386327440255));
#6164=CARTESIAN_POINT('Ctrl Pts',(183.941587367144,35.,6.30854973630244));
#6165=CARTESIAN_POINT('Ctrl Pts',(183.946003354294,35.,5.83162422873126));
#6166=CARTESIAN_POINT('',(184.,35.,0.));
#6167=CARTESIAN_POINT('Origin',(156.,49.,8.));
#6168=CARTESIAN_POINT('Ctrl Pts',(181.667890676754,37.2737119676904,8.));
#6169=CARTESIAN_POINT('Ctrl Pts',(181.974263430434,36.9523898924629,8.));
#6170=CARTESIAN_POINT('Ctrl Pts',(182.271552717037,36.6215018559916,8.));
#6171=CARTESIAN_POINT('Ctrl Pts',(182.837203794954,35.9007967977578,8.));
#6172=CARTESIAN_POINT('Ctrl Pts',(183.128758753871,35.475688585275,8.));
#6173=CARTESIAN_POINT('Ctrl Pts',(183.368772894519,34.999999999999,8.));
#6174=CARTESIAN_POINT('Ctrl Pts',(183.897890720421,32.,11.0277766514379));
#6175=CARTESIAN_POINT('Ctrl Pts',(183.908476258216,32.,9.88454121758138));
#6176=CARTESIAN_POINT('Ctrl Pts',(183.933198048223,32.7822331288304,7.21459408111487));
#6177=CARTESIAN_POINT('Ctrl Pts',(183.948579057724,35.1094518511976,5.5534489026464));
#6178=CARTESIAN_POINT('Ctrl Pts',(183.951893158078,36.5911484250779,5.19552689342517));
#6179=CARTESIAN_POINT('Ctrl Pts',(183.897890720421,32.8975979010257,11.0277766514379));
#6180=CARTESIAN_POINT('Ctrl Pts',(183.906848467244,32.8965695980516,10.0562409853862));
#6181=CARTESIAN_POINT('Ctrl Pts',(183.92786931383,33.5598355037628,7.78441731032418));
#6182=CARTESIAN_POINT('Ctrl Pts',(183.94105067019,35.5403566750075,6.36777674722119));
#6183=CARTESIAN_POINT('Ctrl Pts',(183.94386106412,36.80071300929,6.06299103161509));
#6184=CARTESIAN_POINT('Ctrl Pts',(183.144438752334,34.4514631268444,11.0208002281669));
#6185=CARTESIAN_POINT('Ctrl Pts',(183.152499885901,34.448790086954,10.3444760457849));
#6186=CARTESIAN_POINT('Ctrl Pts',(183.171343341433,34.905148868596,8.76122121233146));
#6187=CARTESIAN_POINT('Ctrl Pts',(183.183090568948,36.2839134347555,7.77152178690107));
#6188=CARTESIAN_POINT('Ctrl Pts',(183.185625354358,37.1635876050048,7.55816920506391));
#6189=CARTESIAN_POINT('Ctrl Pts',(181.571188883105,35.,11.006233066007));
#6190=CARTESIAN_POINT('Ctrl Pts',(181.581029357879,34.9988031377618,10.4350067310519));
#6191=CARTESIAN_POINT('Ctrl Pts',(181.603998038734,35.3874005905622,9.09836594332551));
#6192=CARTESIAN_POINT('Ctrl Pts',(181.618277315131,36.5524153149342,8.26377751595704));
#6193=CARTESIAN_POINT('Ctrl Pts',(181.621361391319,37.2941596483767,8.08421682634416));
#6194=CARTESIAN_POINT('Ctrl Pts',(180.898019313572,35.,11.));
#6195=CARTESIAN_POINT('Ctrl Pts',(180.908604851367,35.,10.4283822830717));
#6196=CARTESIAN_POINT('Ctrl Pts',(180.933326641373,35.3911165644152,9.09340871483851));
#6197=CARTESIAN_POINT('Ctrl Pts',(180.948707650874,36.5547259255988,8.26283612560427));
#6198=CARTESIAN_POINT('Ctrl Pts',(180.952021751228,37.2955742125389,8.08387512099366));
#6199=CARTESIAN_POINT('Origin',(180.898019313572,38.,11.));
#6200=CARTESIAN_POINT('',(183.897890720421,32.,11.0277766514379));
#6201=CARTESIAN_POINT('Origin',(180.898019313572,32.,11.));
#6202=CARTESIAN_POINT('Origin',(183.897890720421,38.,11.0277766514379));
#6203=CARTESIAN_POINT('Origin',(156.,-35.,5.));
#6204=CARTESIAN_POINT('',(131.180652708018,-38.,8.));
#6205=CARTESIAN_POINT('',(128.20233103298,-38.36,5.));
#6206=CARTESIAN_POINT('Origin',(131.180652708018,-38.,5.));
#6207=CARTESIAN_POINT('',(183.79766896702,-38.36,5.));
#6208=CARTESIAN_POINT('Origin',(156.,-35.,5.));
#6209=CARTESIAN_POINT('',(180.819347291982,-38.,8.));
#6210=CARTESIAN_POINT('Origin',(180.819347291982,-38.,5.));
#6211=CARTESIAN_POINT('Origin',(156.,-35.,8.));
#6212=CARTESIAN_POINT('Ctrl Pts',(128.131421846764,-37.7096774193548,5.02816182430651));
#6213=CARTESIAN_POINT('Ctrl Pts',(128.152459235224,-37.926043434088,5.00937844175291));
#6214=CARTESIAN_POINT('Ctrl Pts',(128.176122803378,-38.1431762825264,5.));
#6215=CARTESIAN_POINT('Ctrl Pts',(128.20233103298,-38.36,5.));
#6216=CARTESIAN_POINT('Ctrl Pts',(128.139739095352,-37.7952189272299,5.91625914580451));
#6217=CARTESIAN_POINT('Ctrl Pts',(128.158628084866,-37.9830850669534,5.90163360405695));
#6218=CARTESIAN_POINT('Ctrl Pts',(128.179661431525,-38.1717572674893,5.89534108170859));
#6219=CARTESIAN_POINT('Ctrl Pts',(128.20233103298,-38.36,5.89759790102566));
#6220=CARTESIAN_POINT('Ctrl Pts',(128.894568928654,-37.8713539969118,7.45412541158965));
#6221=CARTESIAN_POINT('Ctrl Pts',(128.91170554589,-38.0040028278317,7.44649047075611));
#6222=CARTESIAN_POINT('Ctrl Pts',(128.93029664544,-38.1370148419096,7.4456515712285));
#6223=CARTESIAN_POINT('Ctrl Pts',(128.950298064189,-38.2695906484878,7.45151809910225));
#6224=CARTESIAN_POINT('Ctrl Pts',(130.451267943487,-37.7738335502611,8.00784297571193));
#6225=CARTESIAN_POINT('Ctrl Pts',(130.469571415126,-37.8759649512522,8.00001814579435));
#6226=CARTESIAN_POINT('Ctrl Pts',(130.48991410944,-37.978663056327,7.99737324321024));
#6227=CARTESIAN_POINT('Ctrl Pts',(130.512318886995,-38.0807838110923,8.00000000000001));
#6228=CARTESIAN_POINT('Ctrl Pts',(131.11734093461,-37.7096774193548,8.01408091215325));
#6229=CARTESIAN_POINT('Ctrl Pts',(131.136124317164,-37.8062693902184,8.0046892208764));
#6230=CARTESIAN_POINT('Ctrl Pts',(131.157252503016,-37.9032036975574,8.00000000000001));
#6231=CARTESIAN_POINT('Ctrl Pts',(131.180652708018,-38.,8.00000000000001));
#6232=CARTESIAN_POINT('',(131.11734093461,-37.7096774193548,8.01408091215326));
#6233=CARTESIAN_POINT('Ctrl Pts',(131.180652708018,-38.,8.00000000000001));
#6234=CARTESIAN_POINT('Ctrl Pts',(131.157252503016,-37.9032036975574,8.00000000000001));
#6235=CARTESIAN_POINT('Ctrl Pts',(131.136124317164,-37.8062693902184,8.0046892208764));
#6236=CARTESIAN_POINT('Ctrl Pts',(131.11734093461,-37.7096774193548,8.01408091215325));
#6237=CARTESIAN_POINT('',(128.131421846764,-37.7096774193548,5.02816182430651));
#6238=CARTESIAN_POINT('Origin',(131.11734093461,-37.4193548387097,5.02816182430651));
#6239=CARTESIAN_POINT('Ctrl Pts',(128.131421846764,-37.7096774193548,5.02816182430651));
#6240=CARTESIAN_POINT('Ctrl Pts',(128.152459235224,-37.926043434088,5.00937844175291));
#6241=CARTESIAN_POINT('Ctrl Pts',(128.176122803378,-38.1431762825264,5.));
#6242=CARTESIAN_POINT('Ctrl Pts',(128.20233103298,-38.36,5.));
#6243=CARTESIAN_POINT('Ctrl Pts',(131.11734093461,-37.7096774193548,8.01408091215326));
#6244=CARTESIAN_POINT('Ctrl Pts',(131.076588756525,-37.5001127583042,8.03445700119595));
#6245=CARTESIAN_POINT('Ctrl Pts',(130.822486477689,-36.8777394142145,8.16150814061386));
#6246=CARTESIAN_POINT('Ctrl Pts',(129.756916368741,-35.9426049163746,8.69429319508786));
#6247=CARTESIAN_POINT('Ctrl Pts',(127.671636697566,-35.1800834699449,9.73693303067528));
#6248=CARTESIAN_POINT('Ctrl Pts',(125.987714439348,-35.,10.5788941597843));
#6249=CARTESIAN_POINT('Ctrl Pts',(125.145502758917,-35.,11.));
#6250=CARTESIAN_POINT('Ctrl Pts',(130.229243613112,-37.7952189272299,8.00576366356483));
#6251=CARTESIAN_POINT('Ctrl Pts',(130.202303508807,-37.6462990978492,8.01387139589604));
#6252=CARTESIAN_POINT('Ctrl Pts',(130.035901503225,-37.1878650592641,8.06332025121927));
#6253=CARTESIAN_POINT('Ctrl Pts',(129.236458211218,-36.2429002783718,8.41304981555658));
#6254=CARTESIAN_POINT('Ctrl Pts',(127.431915327519,-35.2514546514263,9.49424407278561));
#6255=CARTESIAN_POINT('Ctrl Pts',(125.907503803117,-35.,10.4986835235528));
#6256=CARTESIAN_POINT('Ctrl Pts',(125.145502758917,-35.,11.));
#6257=CARTESIAN_POINT('Ctrl Pts',(128.69137689806,-37.8713540986491,7.25093442734691));
#6258=CARTESIAN_POINT('Ctrl Pts',(128.687275356584,-37.7745511646802,7.25754878799169));
#6259=CARTESIAN_POINT('Ctrl Pts',(128.667694768037,-37.4546169089802,7.29289324516655));
#6260=CARTESIAN_POINT('Ctrl Pts',(128.321536446058,-36.4828470073741,7.69451037570431));
#6261=CARTESIAN_POINT('Ctrl Pts',(127.009479360979,-35.3039679777576,9.07589627680508));
#6262=CARTESIAN_POINT('Ctrl Pts',(125.767135189712,-35.,10.3583149101475));
#6263=CARTESIAN_POINT('Ctrl Pts',(125.145502758917,-35.,11.));
#6264=CARTESIAN_POINT('Ctrl Pts',(128.137659783205,-37.7738335502611,5.69423481543001));
#6265=CARTESIAN_POINT('Ctrl Pts',(128.126276420232,-37.6091470033402,5.72485515984047));
#6266=CARTESIAN_POINT('Ctrl Pts',(128.056978238003,-37.1082707099995,5.91366148966411));
#6267=CARTESIAN_POINT('Ctrl Pts',(127.660173748571,-36.1672395340187,6.78108593159827));
#6268=CARTESIAN_POINT('Ctrl Pts',(126.589351201994,-35.2341452946653,8.65501989450532));
#6269=CARTESIAN_POINT('Ctrl Pts',(125.626766576306,-35.,10.2179462967423));
#6270=CARTESIAN_POINT('Ctrl Pts',(125.145502758917,-35.,11.));
#6271=CARTESIAN_POINT('Ctrl Pts',(128.131421846764,-37.7096774193548,5.02816182430651));
#6272=CARTESIAN_POINT('Ctrl Pts',(128.111045757721,-37.5001127583042,5.0689140023919));
#6273=CARTESIAN_POINT('Ctrl Pts',(127.983994618303,-36.8777394142145,5.32301628122771));
#6274=CARTESIAN_POINT('Ctrl Pts',(127.451209563829,-35.9426049163746,6.38858639017571));
#6275=CARTESIAN_POINT('Ctrl Pts',(126.408569728242,-35.1800834699449,8.47386606135057));
#6276=CARTESIAN_POINT('Ctrl Pts',(125.566608599133,-35.,10.1577883195686));
#6277=CARTESIAN_POINT('Ctrl Pts',(125.145502758917,-35.,11.));
#6278=CARTESIAN_POINT('',(125.145502758917,-35.,11.));
#6279=CARTESIAN_POINT('Origin',(125.145502758917,-38.,11.));
#6280=CARTESIAN_POINT('Origin',(125.145502758917,-38.,11.));
#6281=CARTESIAN_POINT('Ctrl Pts',(180.973049661459,-35.9197434605539,8.83839579707758));
#6282=CARTESIAN_POINT('Ctrl Pts',(181.024369346261,-36.4719169174759,8.30700228705497));
#6283=CARTESIAN_POINT('Ctrl Pts',(181.00314731485,-37.2397005666917,8.));
#6284=CARTESIAN_POINT('Ctrl Pts',(180.819347291982,-38.,8.));
#6285=CARTESIAN_POINT('Ctrl Pts',(181.888531321851,-35.8976563985753,8.85965165652495));
#6286=CARTESIAN_POINT('Ctrl Pts',(181.917708840364,-36.4582452641848,8.30800657542114));
#6287=CARTESIAN_POINT('Ctrl Pts',(181.883286339303,-37.2926975054263,7.971937985194));
#6288=CARTESIAN_POINT('Ctrl Pts',(181.710459053346,-38.1077117481231,8.));
#6289=CARTESIAN_POINT('Ctrl Pts',(183.471901157116,-35.3139801735237,8.32960849046661));
#6290=CARTESIAN_POINT('Ctrl Pts',(183.466030118439,-36.0687832506354,7.63040959063072));
#6291=CARTESIAN_POINT('Ctrl Pts',(183.409166117026,-37.1880560548143,7.20299655425038));
#6292=CARTESIAN_POINT('Ctrl Pts',(183.253095761512,-38.2941755608114,7.24651557480386));
#6293=CARTESIAN_POINT('Ctrl Pts',(183.991916857942,-34.1758212771931,7.17205274358105));
#6294=CARTESIAN_POINT('Ctrl Pts',(184.021762067457,-35.2769187438743,6.2180368164864));
#6295=CARTESIAN_POINT('Ctrl Pts',(183.983057240361,-36.8243680976585,5.66035404348166));
#6296=CARTESIAN_POINT('Ctrl Pts',(183.79766896702,-38.36,5.67319842576924));
#6297=CARTESIAN_POINT('Ctrl Pts',(183.969815620835,-33.7002253516408,6.67679159415515));
#6298=CARTESIAN_POINT('Ctrl Pts',(184.027293667812,-34.9370938951461,5.61400457410994));
#6299=CARTESIAN_POINT('Ctrl Pts',(184.003524992632,-36.6569292693893,5.));
#6300=CARTESIAN_POINT('Ctrl Pts',(183.79766896702,-38.36,5.));
#6301=CARTESIAN_POINT('',(181.667890676754,-37.2737119676905,8.));
#6302=CARTESIAN_POINT('',(180.951927410069,-37.2748094218035,8.08896949084808));
#6303=CARTESIAN_POINT('Ctrl Pts',(181.666636694743,-37.2729596773495,7.99687411834348));
#6304=CARTESIAN_POINT('Ctrl Pts',(181.569302349961,-37.2762121398385,8.02134483314431));
#6305=CARTESIAN_POINT('Ctrl Pts',(181.470885453719,-37.2782472631398,8.04110399082257));
#6306=CARTESIAN_POINT('Ctrl Pts',(181.371712379837,-37.2790308976767,8.05596775956708));
#6307=CARTESIAN_POINT('Ctrl Pts',(181.27436640165,-37.2798000950764,8.07055768858045));
#6308=CARTESIAN_POINT('Ctrl Pts',(181.176291132015,-37.2793632927185,8.08043120267881));
#6309=CARTESIAN_POINT('Ctrl Pts',(181.077788864619,-37.2776661013203,8.08537023158407));
#6310=CARTESIAN_POINT('Ctrl Pts',(181.0399937172,-37.2770148919544,8.08726532832156));
#6311=CARTESIAN_POINT('Ctrl Pts',(181.002135693703,-37.2761779038092,8.08843345948832));
#6312=CARTESIAN_POINT('Ctrl Pts',(180.964231951489,-37.2751512711449,8.08886040524177));
#6313=CARTESIAN_POINT('Ctrl Pts',(180.960130633245,-37.2750401858792,8.08890660227419));
#6314=CARTESIAN_POINT('Ctrl Pts',(180.956029091187,-37.2749268986846,8.08894411433519));
#6315=CARTESIAN_POINT('Ctrl Pts',(180.951927347206,-37.2748114061892,8.08897292638101));
#6316=CARTESIAN_POINT('Ctrl Pts',(180.948784580753,-37.2752662540447,8.09156800850377));
#6317=CARTESIAN_POINT('Ctrl Pts',(180.920314453382,-37.512739598246,8.03142446135659));
#6318=CARTESIAN_POINT('Ctrl Pts',(180.87815153677,-37.7567528377248,8.));
#6319=CARTESIAN_POINT('Ctrl Pts',(180.819347291982,-38.,8.));
#6320=CARTESIAN_POINT('',(184.,-35.0000000018351,5.8038475754014));
#6321=CARTESIAN_POINT('Ctrl Pts',(183.79766896702,-38.36,5.));
#6322=CARTESIAN_POINT('Ctrl Pts',(183.938441824961,-37.1953698498218,5.));
#6323=CARTESIAN_POINT('Ctrl Pts',(183.994063543363,-36.0228998990979,5.28713246166602));
#6324=CARTESIAN_POINT('Ctrl Pts',(183.996782032333,-35.0023997001806,5.80856086039142));
#6325=CARTESIAN_POINT('',(183.402520572671,-35.,8.));
#6326=CARTESIAN_POINT('Ctrl Pts',(184.,-35.,5.80384757729336));
#6327=CARTESIAN_POINT('Ctrl Pts',(184.,-35.,6.26767582544512));
#6328=CARTESIAN_POINT('Ctrl Pts',(183.917463444079,-35.,6.72592757665807));
#6329=CARTESIAN_POINT('Ctrl Pts',(183.671800315476,-35.,7.45588656812286));
#6330=CARTESIAN_POINT('Ctrl Pts',(183.547885506158,-35.,7.73310336009194));
#6331=CARTESIAN_POINT('Ctrl Pts',(183.402520572671,-35.,8.00000000000001));
#6332=CARTESIAN_POINT('Ctrl Pts',(183.402520572671,-35.,8.));
#6333=CARTESIAN_POINT('Ctrl Pts',(183.212882493681,-35.3969969877486,8.));
#6334=CARTESIAN_POINT('Ctrl Pts',(182.944508993243,-35.8456903827968,8.00000000002023));
#6335=CARTESIAN_POINT('Ctrl Pts',(182.2724761698,-36.6776120047321,8.00000000002023));
#6336=CARTESIAN_POINT('Ctrl Pts',(181.971845249822,-36.9899807223263,8.));
#6337=CARTESIAN_POINT('Ctrl Pts',(181.667890676754,-37.2737119676906,8.));
#6338=CARTESIAN_POINT('Origin',(125.145502758917,-38.,0.));
#6339=CARTESIAN_POINT('',(125.145502758917,-35.,0.));
#6340=CARTESIAN_POINT('',(128.131421846764,-37.7096774193548,0.));
#6341=CARTESIAN_POINT('Origin',(124.,-38.,11.));
#6342=CARTESIAN_POINT('',(124.,-38.,8.));
#6343=CARTESIAN_POINT('',(180.898019313572,-35.,11.));
#6344=CARTESIAN_POINT('Origin',(180.898019313572,-38.,11.));
#6345=CARTESIAN_POINT('',(124.,-35.,11.));
#6346=CARTESIAN_POINT('Origin',(156.,-49.,8.));
#6347=CARTESIAN_POINT('',(183.368772894521,-35.,7.99999999999765));
#6348=CARTESIAN_POINT('',(0.,-35.,8.));
#6349=CARTESIAN_POINT('Ctrl Pts',(183.368772894519,-34.999999999999,8.));
#6350=CARTESIAN_POINT('Ctrl Pts',(183.128758753872,-35.4756885852746,8.));
#6351=CARTESIAN_POINT('Ctrl Pts',(182.837203794954,-35.9007967977573,8.));
#6352=CARTESIAN_POINT('Ctrl Pts',(182.271552980708,-36.6215015200439,8.));
#6353=CARTESIAN_POINT('Ctrl Pts',(181.974263989935,-36.9523893056604,8.));
#6354=CARTESIAN_POINT('Ctrl Pts',(181.667890676754,-37.2737119676906,8.));
#6355=CARTESIAN_POINT('Origin',(156.,-49.,8.));
#6356=CARTESIAN_POINT('',(152.,-50.,8.));
#6357=CARTESIAN_POINT('Origin',(156.,-50.,8.));
#6358=CARTESIAN_POINT('Ctrl Pts',(180.898019313572,-35.,11.));
#6359=CARTESIAN_POINT('Ctrl Pts',(180.908604851367,-35.,10.4283822830717));
#6360=CARTESIAN_POINT('Ctrl Pts',(180.933326641373,-35.3911165644152,9.09340871483843));
#6361=CARTESIAN_POINT('Ctrl Pts',(180.948707650874,-36.5547259255989,8.2628361256042));
#6362=CARTESIAN_POINT('Ctrl Pts',(180.952021751228,-37.2955742125391,8.08387512099361));
#6363=CARTESIAN_POINT('Ctrl Pts',(181.795578739617,-35.,11.0083107546761));
#6364=CARTESIAN_POINT('Ctrl Pts',(181.805136018515,-34.9983721392498,10.4383579957919));
#6365=CARTESIAN_POINT('Ctrl Pts',(181.827506908354,-35.3867659352872,9.10160449078975));
#6366=CARTESIAN_POINT('Ctrl Pts',(181.841477858758,-36.553089478282,8.26375258453703));
#6367=CARTESIAN_POINT('Ctrl Pts',(181.844474604683,-37.2936881269894,8.08433072812761));
#6368=CARTESIAN_POINT('Ctrl Pts',(183.349377359961,-34.246515734274,11.0226978122624));
#6369=CARTESIAN_POINT('Ctrl Pts',(183.357289972444,-34.2439912218348,10.307278215092));
#6370=CARTESIAN_POINT('Ctrl Pts',(183.375789434442,-34.7273862841715,8.63302779348577));
#6371=CARTESIAN_POINT('Ctrl Pts',(183.387325672956,-36.1854736296666,7.58707377292744));
#6372=CARTESIAN_POINT('Ctrl Pts',(183.38981428891,-37.115640232766,7.36157119560973));
#6373=CARTESIAN_POINT('Ctrl Pts',(183.897890720421,-32.6731984257692,11.0277766514379));
#6374=CARTESIAN_POINT('Ctrl Pts',(183.907279447281,-32.6724533308097,10.0123730883188));
#6375=CARTESIAN_POINT('Ctrl Pts',(183.92923478795,-33.3649359383542,7.64065313694788));
#6376=CARTESIAN_POINT('Ctrl Pts',(183.942925420429,-35.431438721091,6.16447437754468));
#6377=CARTESIAN_POINT('Ctrl Pts',(183.94586908761,-36.7483218632372,5.84612499706756));
#6378=CARTESIAN_POINT('Ctrl Pts',(183.897890720421,-32.,11.0277766514379));
#6379=CARTESIAN_POINT('Ctrl Pts',(183.908476258216,-32.,9.88454121758135));
#6380=CARTESIAN_POINT('Ctrl Pts',(183.933198048223,-32.7822331288305,7.21459408111476));
#6381=CARTESIAN_POINT('Ctrl Pts',(183.948579057724,-35.1094518511978,5.55344890264629));
#6382=CARTESIAN_POINT('Ctrl Pts',(183.951893158078,-36.5911484250781,5.19552689342511));
#6383=CARTESIAN_POINT('',(183.946003354294,-35.,5.83162422873126));
#6384=CARTESIAN_POINT('Ctrl Pts',(183.946003354294,-35.,5.83162422873127));
#6385=CARTESIAN_POINT('Ctrl Pts',(183.941587367144,-35.,6.30854973630342));
#6386=CARTESIAN_POINT('Ctrl Pts',(183.851877965836,-35.,6.83863274402651));
#6387=CARTESIAN_POINT('Ctrl Pts',(183.555890991522,-35.,7.61467203113213));
#6388=CARTESIAN_POINT('Ctrl Pts',(183.466406037598,-35.,7.81137594025207));
#6389=CARTESIAN_POINT('Ctrl Pts',(183.36877289452,-35.,7.99999999999715));
#6390=CARTESIAN_POINT('',(183.897890720421,-32.,11.0277766514379));
#6391=CARTESIAN_POINT('Origin',(183.897890720421,-38.,11.0277766514379));
#6392=CARTESIAN_POINT('Origin',(180.898019313572,-32.,11.));
#6393=CARTESIAN_POINT('Origin',(180.542507983541,-32.,49.3951347106504));
#6394=CARTESIAN_POINT('',(183.509279157931,-32.,52.9977281876795));
#6395=CARTESIAN_POINT('',(183.542379390391,-32.,49.4229113620883));
#6396=CARTESIAN_POINT('',(180.509407751081,-35.,52.9699515362416));
#6397=CARTESIAN_POINT('Origin',(180.509407751081,-32.,52.9699515362416));
#6398=CARTESIAN_POINT('',(180.542507983541,-35.,49.3951347106504));
#6399=CARTESIAN_POINT('Origin',(180.426077796767,22.9619250064101,61.969565756791));
#6400=CARTESIAN_POINT('',(183.472204154205,15.4757638065838,57.0018193155226));
#6401=CARTESIAN_POINT('',(183.509279157931,22.9619250064101,52.9977281876795));
#6402=CARTESIAN_POINT('Origin',(183.425949203617,22.9619250064101,61.9973424082289));
#6403=CARTESIAN_POINT('',(180.481631099643,22.9619250064101,55.9698229430914));
#6404=CARTESIAN_POINT('Origin',(180.509407751081,22.9619250064101,52.9699515362416));
#6405=CARTESIAN_POINT('',(180.456854989517,17.9668779442357,58.6456286919431));
#6406=CARTESIAN_POINT('Origin',(180.426077796767,22.9619250064101,61.969565756791));
#6407=CARTESIAN_POINT('Ctrl Pts',(180.456855041398,17.9668744188066,58.6456339902688));
#6408=CARTESIAN_POINT('Ctrl Pts',(180.464169860625,17.9668900378147,58.6456782485915));
#6409=CARTESIAN_POINT('Ctrl Pts',(180.471484765196,17.9668833841778,58.6457076852037));
#6410=CARTESIAN_POINT('Ctrl Pts',(180.875311709676,17.9652864766128,58.6465145041401));
#6411=CARTESIAN_POINT('Ctrl Pts',(181.267746602967,17.8982906281074,58.6037468164134));
#6412=CARTESIAN_POINT('Ctrl Pts',(181.993556182758,17.6431112722523,58.4372902978833));
#6413=CARTESIAN_POINT('Ctrl Pts',(182.320780158277,17.4591760990087,58.3164001965527));
#6414=CARTESIAN_POINT('Ctrl Pts',(182.872438697285,16.9974183098841,58.0116647840574));
#6415=CARTESIAN_POINT('Ctrl Pts',(183.091599797094,16.7240114613764,57.8307336627257));
#6416=CARTESIAN_POINT('Ctrl Pts',(183.391916275035,16.1229170096583,57.432110771519));
#6417=CARTESIAN_POINT('Ctrl Pts',(183.470200344055,15.8009765931121,57.218230310496));
#6418=CARTESIAN_POINT('Ctrl Pts',(183.472204154205,15.4757638065857,57.0018193155196));
#6419=CARTESIAN_POINT('Origin',(180.509407751081,17.5,52.9699515362416));
#6420=CARTESIAN_POINT('',(183.509279157931,32.,52.9977281876795));
#6421=CARTESIAN_POINT('',(180.481631099643,32.,55.9698229430914));
#6422=CARTESIAN_POINT('Origin',(180.509407751081,32.,52.9699515362416));
#6423=CARTESIAN_POINT('',(180.481631099643,17.5,55.9698229430914));
#6424=CARTESIAN_POINT('',(183.509279157931,17.5,52.9977281876795));
#6425=CARTESIAN_POINT('Ctrl Pts',(180.456854989517,17.9668779442357,58.6456286919431));
#6426=CARTESIAN_POINT('Ctrl Pts',(180.459728353753,17.5538362749007,59.2663537452259));
#6427=CARTESIAN_POINT('Ctrl Pts',(180.462961268117,17.2579323958192,59.9647514337378));
#6428=CARTESIAN_POINT('Ctrl Pts',(180.466333696842,17.0993058558373,60.6932880299539));
#6429=CARTESIAN_POINT('Ctrl Pts',(181.357372224078,17.9707236015583,58.6481877715177));
#6430=CARTESIAN_POINT('Ctrl Pts',(181.359700243583,17.5578731302105,59.2670196267812));
#6431=CARTESIAN_POINT('Ctrl Pts',(181.362326456225,17.2603980067746,59.9666372804095));
#6432=CARTESIAN_POINT('Ctrl Pts',(181.365055554869,17.1010357845145,60.6936647088526));
#6433=CARTESIAN_POINT('Ctrl Pts',(182.919937109513,17.3457188040812,58.23228045658));
#6434=CARTESIAN_POINT('Ctrl Pts',(182.920639258236,16.8800887242898,58.9295321606114));
#6435=CARTESIAN_POINT('Ctrl Pts',(182.921424127829,16.5458858994944,59.7141124557901));
#6436=CARTESIAN_POINT('Ctrl Pts',(182.922246255174,16.3658079346786,60.5335743996686));
#6437=CARTESIAN_POINT('Ctrl Pts',(183.47224362268,16.0316349538676,57.357827831654));
#6438=CARTESIAN_POINT('Ctrl Pts',(183.472236359704,15.4580713295682,58.2190205931141));
#6439=CARTESIAN_POINT('Ctrl Pts',(183.472252068947,15.0472514462844,59.1873279691006));
#6440=CARTESIAN_POINT('Ctrl Pts',(183.47224362268,14.826606833477,60.1984249895329));
#6441=CARTESIAN_POINT('Ctrl Pts',(183.47224362268,15.4693544131485,56.9836601598598));
#6442=CARTESIAN_POINT('Ctrl Pts',(183.47224362268,14.8497919091461,57.9147078318549));
#6443=CARTESIAN_POINT('Ctrl Pts',(183.47224362268,14.4059360905238,58.9622594629304));
#6444=CARTESIAN_POINT('Ctrl Pts',(183.47224362268,14.1679962805509,60.0550175178582));
#6445=CARTESIAN_POINT('',(180.466333696842,17.0993058558373,60.6932880299539));
#6446=CARTESIAN_POINT('Origin',(180.47224362268,22.9619250064101,61.9699932191321));
#6447=CARTESIAN_POINT('',(183.47224362268,14.1679962805509,60.0550175178582));
#6448=CARTESIAN_POINT('Origin',(180.47224362268,14.1679962805509,60.0550175178582));
#6449=CARTESIAN_POINT('',(183.47224362268,15.4601255574769,56.9975567301459));
#6450=CARTESIAN_POINT('Origin',(183.47224362268,22.9619250064101,61.9699932191321));
#6451=CARTESIAN_POINT('Ctrl Pts',(183.47224362268,15.460125717566,56.99755680507));
#6452=CARTESIAN_POINT('Ctrl Pts',(183.472243622256,15.4633487844854,56.9975568030941));
#6453=CARTESIAN_POINT('Ctrl Pts',(183.472239876315,15.4665745708394,56.9979465749962));
#6454=CARTESIAN_POINT('Ctrl Pts',(183.472230569335,15.4696494558241,56.9989155565643));
#6455=CARTESIAN_POINT('Ctrl Pts',(183.472223954011,15.4718350589064,56.9996043007328));
#6456=CARTESIAN_POINT('Ctrl Pts',(183.472214729775,15.4738784948292,57.0005647940433));
#6457=CARTESIAN_POINT('Ctrl Pts',(183.472202682799,15.4757640046251,57.0018195104561));
#6458=CARTESIAN_POINT('Ctrl Pts',(180.466333696842,17.0993058558373,60.6932880299539));
#6459=CARTESIAN_POINT('Ctrl Pts',(180.462827663279,16.6183159756739,62.9022409648325));
#6460=CARTESIAN_POINT('Ctrl Pts',(180.456117112077,14.7896202235287,67.1301787480821));
#6461=CARTESIAN_POINT('Ctrl Pts',(180.448438324107,9.85407602191408,71.9681476145139));
#6462=CARTESIAN_POINT('Ctrl Pts',(180.444297004961,3.45518438994196,74.57735797057));
#6463=CARTESIAN_POINT('Ctrl Pts',(180.444293007696,-3.45535478712963,74.5798764205847));
#6464=CARTESIAN_POINT('Ctrl Pts',(180.448441988675,-9.85267395691086,71.9658387779471));
#6465=CARTESIAN_POINT('Ctrl Pts',(180.456114870671,-14.7904585682235,67.1315909309643));
#6466=CARTESIAN_POINT('Ctrl Pts',(180.462827663279,-16.6183159756739,62.9022409648325));
#6467=CARTESIAN_POINT('Ctrl Pts',(180.466333696842,-17.0993058558373,60.6932880299539));
#6468=CARTESIAN_POINT('Ctrl Pts',(181.365055554869,17.1010357845145,60.6936647088526));
#6469=CARTESIAN_POINT('Ctrl Pts',(181.362218338067,16.6208107320077,62.9041865999037));
#6470=CARTESIAN_POINT('Ctrl Pts',(181.356777150885,14.7954594744657,67.1334068171006));
#6471=CARTESIAN_POINT('Ctrl Pts',(181.35054979597,9.85934073046915,71.9768075336286));
#6472=CARTESIAN_POINT('Ctrl Pts',(181.347185400725,3.45736101376534,74.5882859850751));
#6473=CARTESIAN_POINT('Ctrl Pts',(181.347183692439,-3.45785563298963,74.5914144228182));
#6474=CARTESIAN_POINT('Ctrl Pts',(181.350551527384,-9.85766669730974,71.9740201461265));
#6475=CARTESIAN_POINT('Ctrl Pts',(181.356775216638,-14.7971451523738,67.1347728987079));
#6476=CARTESIAN_POINT('Ctrl Pts',(181.362218338067,-16.6208107320077,62.9041865999037));
#6477=CARTESIAN_POINT('Ctrl Pts',(181.365055554869,-17.1010357845145,60.6936647088526));
#6478=CARTESIAN_POINT('Ctrl Pts',(182.922243752064,16.3658046786719,60.5335736906977));
#6479=CARTESIAN_POINT('Ctrl Pts',(182.921389054663,15.9071160601721,62.6479991065062));
#6480=CARTESIAN_POINT('Ctrl Pts',(182.919754407863,14.1594944560602,66.6966525066034));
#6481=CARTESIAN_POINT('Ctrl Pts',(182.917876131385,9.43644362697149,71.3316844154431));
#6482=CARTESIAN_POINT('Ctrl Pts',(182.916863279067,3.30915221594224,73.8324898890446));
#6483=CARTESIAN_POINT('Ctrl Pts',(182.916861444842,-3.30927917380312,73.8348409593045));
#6484=CARTESIAN_POINT('Ctrl Pts',(182.917877699306,-9.43511943897599,71.329525787935));
#6485=CARTESIAN_POINT('Ctrl Pts',(182.919753921885,-14.1602031813203,66.6980124501267));
#6486=CARTESIAN_POINT('Ctrl Pts',(182.921389054663,-15.9071160601721,62.6479991065062));
#6487=CARTESIAN_POINT('Ctrl Pts',(182.922243752064,-16.3658046786719,60.5335736906977));
#6488=CARTESIAN_POINT('Ctrl Pts',(183.47224362268,14.826606833477,60.1984249895329));
#6489=CARTESIAN_POINT('Ctrl Pts',(183.472252403561,14.4100919837911,62.1136233600875));
#6490=CARTESIAN_POINT('Ctrl Pts',(183.472249275606,12.824852883573,65.7803651712171));
#6491=CARTESIAN_POINT('Ctrl Pts',(183.472264206913,8.54564648381244,69.9763019277475));
#6492=CARTESIAN_POINT('Ctrl Pts',(183.472262740902,2.99650804402197,72.2398310923833));
#6493=CARTESIAN_POINT('Ctrl Pts',(183.472267398591,-2.99657429455144,72.2418653039269));
#6494=CARTESIAN_POINT('Ctrl Pts',(183.472260521092,-8.5444936796726,69.974419227184));
#6495=CARTESIAN_POINT('Ctrl Pts',(183.472248913357,-12.8253671346527,65.7816026321006));
#6496=CARTESIAN_POINT('Ctrl Pts',(183.472252403561,-14.4100919837911,62.1136233600875));
#6497=CARTESIAN_POINT('Ctrl Pts',(183.47224362268,-14.826606833477,60.1984249895329));
#6498=CARTESIAN_POINT('Ctrl Pts',(183.47224362268,14.1679962805509,60.0550175178582));
#6499=CARTESIAN_POINT('Ctrl Pts',(183.47224362268,13.7694618084156,61.885319704961));
#6500=CARTESIAN_POINT('Ctrl Pts',(183.47224362268,12.2542567566381,65.3885196371233));
#6501=CARTESIAN_POINT('Ctrl Pts',(183.47224362268,8.16480584672881,69.3971813236395));
#6502=CARTESIAN_POINT('Ctrl Pts',(183.47224362268,2.86286706595191,71.5591302478991));
#6503=CARTESIAN_POINT('Ctrl Pts',(183.47224362268,-2.86300825219312,71.5612169942924));
#6504=CARTESIAN_POINT('Ctrl Pts',(183.47224362268,-8.16364413572614,69.3952682595125));
#6505=CARTESIAN_POINT('Ctrl Pts',(183.47224362268,-12.2549513850995,65.3896897487074));
#6506=CARTESIAN_POINT('Ctrl Pts',(183.47224362268,-13.7694618084156,61.885319704961));
#6507=CARTESIAN_POINT('Ctrl Pts',(183.47224362268,-14.1679962805509,60.0550175178582));
#6508=CARTESIAN_POINT('',(180.466333696842,-17.0993058558373,60.6932880299539));
#6509=CARTESIAN_POINT('',(183.47224362268,-14.1679962805509,60.0550175178582));
#6510=CARTESIAN_POINT('Origin',(180.47224362268,-14.1679962805509,60.0550175178582));
#6511=CARTESIAN_POINT('Origin',(183.47224362268,0.,56.9697788880279));
#6512=CARTESIAN_POINT('Origin',(180.47224362268,0.,56.9697788880279));
#6513=CARTESIAN_POINT('Ctrl Pts',(180.466333696842,-17.0993058558373,60.6932880299539));
#6514=CARTESIAN_POINT('Ctrl Pts',(180.462961267011,-17.2579324478525,59.9647511947606));
#6515=CARTESIAN_POINT('Ctrl Pts',(180.459728351634,-17.5538364699809,59.2663532874908));
#6516=CARTESIAN_POINT('Ctrl Pts',(180.456854986689,-17.9668783506978,58.6456280811059));
#6517=CARTESIAN_POINT('Ctrl Pts',(181.365055554869,-17.1010357845145,60.6936647088526));
#6518=CARTESIAN_POINT('Ctrl Pts',(181.36232645533,-17.2603980590491,59.9666370419274));
#6519=CARTESIAN_POINT('Ctrl Pts',(181.359700241865,-17.5578733261006,59.2670191693394));
#6520=CARTESIAN_POINT('Ctrl Pts',(181.357372221785,-17.9707240084164,58.6481871616225));
#6521=CARTESIAN_POINT('Ctrl Pts',(182.922246255174,-16.3658079346786,60.5335743996685));
#6522=CARTESIAN_POINT('Ctrl Pts',(182.921424127559,-16.5458859585642,59.7141121869873));
#6523=CARTESIAN_POINT('Ctrl Pts',(182.92063925772,-16.8800889446273,58.9295316462732));
#6524=CARTESIAN_POINT('Ctrl Pts',(182.919937108823,-17.3457192622232,58.2322797705467));
#6525=CARTESIAN_POINT('Ctrl Pts',(183.47224362268,-14.826606833477,60.1984249895329));
#6526=CARTESIAN_POINT('Ctrl Pts',(183.472252068949,-15.047251518661,59.187327637437));
#6527=CARTESIAN_POINT('Ctrl Pts',(183.472236359702,-15.4580716004586,58.2190199582051));
#6528=CARTESIAN_POINT('Ctrl Pts',(183.47224362268,-16.0316355181454,57.3578269844147));
#6529=CARTESIAN_POINT('Ctrl Pts',(183.47224362268,-14.1679962805509,60.0550175178582));
#6530=CARTESIAN_POINT('Ctrl Pts',(183.47224362268,-14.4059361685737,58.96225910448));
#6531=CARTESIAN_POINT('Ctrl Pts',(183.47224362268,-14.8497922017664,57.9147071452817));
#6532=CARTESIAN_POINT('Ctrl Pts',(183.47224362268,-15.4693550228417,56.9836592436433));
#6533=CARTESIAN_POINT('',(183.47224362268,-15.4601255574769,56.9975567301459));
#6534=CARTESIAN_POINT('Origin',(183.47224362268,-22.9619250064101,61.9699932191321));
#6535=CARTESIAN_POINT('',(180.456855068753,-17.9668783510483,58.6456280813391));
#6536=CARTESIAN_POINT('Origin',(180.47224362268,-22.9619250064101,61.9699932191321));
#6537=CARTESIAN_POINT('',(183.472204154205,-15.4757638065838,57.0018193155226));
#6538=CARTESIAN_POINT('Ctrl Pts',(180.456855068753,-17.9668783510483,58.6456280813391));
#6539=CARTESIAN_POINT('Ctrl Pts',(180.464169869075,-17.9668926591679,58.6456743092186));
#6540=CARTESIAN_POINT('Ctrl Pts',(180.471484145303,-17.9668818389629,58.6457066556687));
#6541=CARTESIAN_POINT('Ctrl Pts',(180.478797763496,-17.9668498954977,58.6457192600464));
#6542=CARTESIAN_POINT('Ctrl Pts',(180.578070855833,-17.9664163034663,58.6458903484901));
#6543=CARTESIAN_POINT('Ctrl Pts',(180.676977830015,-17.9616130352007,58.6431515554912));
#6544=CARTESIAN_POINT('Ctrl Pts',(180.775213368172,-17.9526628202417,58.6376503408695));
#6545=CARTESIAN_POINT('Ctrl Pts',(180.87523702284,-17.943549690441,58.6320489912776));
#6546=CARTESIAN_POINT('Ctrl Pts',(180.974565314722,-17.9301370725114,58.6235836190736));
#6547=CARTESIAN_POINT('Ctrl Pts',(181.072876795846,-17.9126141567353,58.6123787823608));
#6548=CARTESIAN_POINT('Ctrl Pts',(181.172437383241,-17.8948686018158,58.6010315814843));
#6549=CARTESIAN_POINT('Ctrl Pts',(181.270955974619,-17.8729073888473,58.5868747071206));
#6550=CARTESIAN_POINT('Ctrl Pts',(181.368087710061,-17.8468838149634,58.5700080488639));
#6551=CARTESIAN_POINT('Ctrl Pts',(181.457022956091,-17.8230562478413,58.554564688412));
#6552=CARTESIAN_POINT('Ctrl Pts',(181.544795876943,-17.7958223204274,58.5368491259175));
#6553=CARTESIAN_POINT('Ctrl Pts',(181.631124895745,-17.7652713626968,58.5169185212022));
#6554=CARTESIAN_POINT('Ctrl Pts',(181.725234439151,-17.7319669568023,58.4951916426208));
#6555=CARTESIAN_POINT('Ctrl Pts',(181.817159917646,-17.6948871774175,58.4709408717903));
#6556=CARTESIAN_POINT('Ctrl Pts',(181.906575569164,-17.6542232102784,58.4442930581019));
#6557=CARTESIAN_POINT('Ctrl Pts',(181.99615909615,-17.6134828976408,58.4175952138639));
#6558=CARTESIAN_POINT('Ctrl Pts',(182.083224170943,-17.5691445827376,58.388491086226));
#6559=CARTESIAN_POINT('Ctrl Pts',(182.167424720833,-17.5213601095481,58.3570805184098));
#6560=CARTESIAN_POINT('Ctrl Pts',(182.25013097461,-17.4744236611358,58.3262273898202));
#6561=CARTESIAN_POINT('Ctrl Pts',(182.330074149522,-17.424161867348,58.2931486762449));
#6562=CARTESIAN_POINT('Ctrl Pts',(182.406897605853,-17.3706855018434,58.2579162124748));
#6563=CARTESIAN_POINT('Ctrl Pts',(182.472213528813,-17.3252194640436,58.2279612872582));
#6564=CARTESIAN_POINT('Ctrl Pts',(182.535274131469,-17.2774291143008,58.1964490729091));
#6565=CARTESIAN_POINT('Ctrl Pts',(182.595837938797,-17.2273663652658,58.1634125514998));
#6566=CARTESIAN_POINT('Ctrl Pts',(182.668050183894,-17.1676748818037,58.1240220064466));
#6567=CARTESIAN_POINT('Ctrl Pts',(182.736357538825,-17.1050472239898,58.0826594130257));
#6568=CARTESIAN_POINT('Ctrl Pts',(182.80042592618,-17.0396320551764,58.0394232766223));
#6569=CARTESIAN_POINT('Ctrl Pts',(182.804732571366,-17.035234880009,58.036516965001));
#6570=CARTESIAN_POINT('Ctrl Pts',(182.809020051043,-17.0308250966777,58.0336021791574));
#6571=CARTESIAN_POINT('Ctrl Pts',(182.813288258365,-17.026402744861,58.030678945324));
#6572=CARTESIAN_POINT('Ctrl Pts',(182.875945616796,-16.9614825425481,57.9877658213259));
#6573=CARTESIAN_POINT('Ctrl Pts',(182.934453087186,-16.8938562039598,57.9430337528228));
#6574=CARTESIAN_POINT('Ctrl Pts',(182.988728507397,-16.8238623650039,57.896707024575));
#6575=CARTESIAN_POINT('Ctrl Pts',(183.04366780639,-16.7530123848283,57.8498136432871));
#6576=CARTESIAN_POINT('Ctrl Pts',(183.094271276253,-16.6797359604965,57.8012858973768));
#6577=CARTESIAN_POINT('Ctrl Pts',(183.14040883038,-16.6043605384826,57.7513404279431));
#6578=CARTESIAN_POINT('Ctrl Pts',(183.176387827286,-16.5455812614554,57.7123919417435));
#6579=CARTESIAN_POINT('Ctrl Pts',(183.209650168388,-16.4855249573283,57.6725809164522));
#6580=CARTESIAN_POINT('Ctrl Pts',(183.240113291573,-16.4243411280662,57.6320062199135));
#6581=CARTESIAN_POINT('Ctrl Pts',(183.279095707768,-16.3460466773555,57.5800844357336));
#6582=CARTESIAN_POINT('Ctrl Pts',(183.313304429564,-16.2662909288594,57.5271679917355));
#6583=CARTESIAN_POINT('Ctrl Pts',(183.342661685082,-16.1854199607586,57.4734863710623));
#6584=CARTESIAN_POINT('Ctrl Pts',(183.372088662144,-16.1043569294474,57.4196772600839));
#6585=CARTESIAN_POINT('Ctrl Pts',(183.396641398369,-16.0221726384945,57.3650988382935));
#6586=CARTESIAN_POINT('Ctrl Pts',(183.416194188832,-15.9391967318707,57.3099699346756));
#6587=CARTESIAN_POINT('Ctrl Pts',(183.435389595124,-15.857737451516,57.2558486722733));
#6588=CARTESIAN_POINT('Ctrl Pts',(183.449766291803,-15.7755145143301,57.2011963891436));
#6589=CARTESIAN_POINT('Ctrl Pts',(183.459156841502,-15.6928324349362,57.1462155529733));
#6590=CARTESIAN_POINT('Ctrl Pts',(183.467342656943,-15.6207578212171,57.098288329106));
#6591=CARTESIAN_POINT('Ctrl Pts',(183.471739016432,-15.5483339332306,57.0501111947275));
#6592=CARTESIAN_POINT('Ctrl Pts',(183.472202682799,-15.4757640046365,57.0018195104682));
#6593=CARTESIAN_POINT('Ctrl Pts',(183.472202682799,-15.4757640046365,57.0018195104682));
#6594=CARTESIAN_POINT('Ctrl Pts',(183.472211127192,-15.4744423453996,57.000940011793));
#6595=CARTESIAN_POINT('Ctrl Pts',(183.472218262832,-15.4730308628213,57.0001969339396));
#6596=CARTESIAN_POINT('Ctrl Pts',(183.472224092048,-15.4715297601456,56.9995899676826));
#6597=CARTESIAN_POINT('Ctrl Pts',(183.472238137763,-15.4679127966574,56.9981274596038));
#6598=CARTESIAN_POINT('Ctrl Pts',(183.472243622167,-15.4640255998031,56.9975568026889));
#6599=CARTESIAN_POINT('Ctrl Pts',(183.47224362268,-15.4601257175872,56.9975568050799));
#6600=CARTESIAN_POINT('Origin',(180.426077796767,-22.9619250064101,61.969565756791));
#6601=CARTESIAN_POINT('',(180.481631099643,-22.9619250064101,55.9698229430914));
#6602=CARTESIAN_POINT('Origin',(180.426077796767,-22.9619250064101,61.969565756791));
#6603=CARTESIAN_POINT('',(183.509279157931,-22.9619250064101,52.9977281876795));
#6604=CARTESIAN_POINT('Origin',(180.509407751081,-22.9619250064101,52.9699515362416));
#6605=CARTESIAN_POINT('Origin',(183.425949203617,-22.9619250064101,61.9973424082289));
#6606=CARTESIAN_POINT('Origin',(180.509407751081,-11.480962503205,52.9699515362416));
#6607=CARTESIAN_POINT('',(180.481631099643,-32.,55.9698229430914));
#6608=CARTESIAN_POINT('Origin',(180.509407751081,-32.,52.9699515362416));
#6609=CARTESIAN_POINT('',(183.509279157931,-11.480962503205,52.9977281876795));
#6610=CARTESIAN_POINT('',(180.481631099643,-11.480962503205,55.9698229430914));
#6611=CARTESIAN_POINT('Origin',(180.542507983541,32.,49.3951347106504));
#6612=CARTESIAN_POINT('Origin',(180.509407751081,32.,52.9699515362416));
#6613=CARTESIAN_POINT('',(183.542379390391,32.,49.4229113620883));
#6614=CARTESIAN_POINT('Origin',(180.509407751081,32.,52.9699515362416));
#6615=CARTESIAN_POINT('Origin',(180.509407751081,32.,52.9699515362416));
#6616=CARTESIAN_POINT('Origin',(180.509407751081,-32.,52.9699515362416));
#6617=CARTESIAN_POINT('Origin',(180.509407751081,-32.,52.9699515362416));
#6618=CARTESIAN_POINT('Origin',(156.,-35.,0.));
#6619=CARTESIAN_POINT('',(184.,-35.,0.));
#6620=CARTESIAN_POINT('Origin',(92.,-35.,41.));
#6621=CARTESIAN_POINT('',(60.,-35.,11.));
#6622=CARTESIAN_POINT('',(158.47224362268,-35.,52.7659032476128));
#6623=CARTESIAN_POINT('',(137.703021578879,-35.,52.5735951906642));
#6624=CARTESIAN_POINT('',(158.47224362268,-35.,37.));
#6625=CARTESIAN_POINT('',(158.47224362268,-35.,74.9975567301459));
#6626=CARTESIAN_POINT('',(158.47224362268,-35.,37.));
#6627=CARTESIAN_POINT('',(31.47224362268,-35.,82.));
#6628=CARTESIAN_POINT('Origin',(137.703021578879,-32.,52.5735951906642));
#6629=CARTESIAN_POINT('',(158.47224362268,-32.,55.7660318462753));
#6630=CARTESIAN_POINT('',(137.675244927441,-32.,55.573466597514));
#6631=CARTESIAN_POINT('Origin',(158.47224362268,-32.,52.7659032476128));
#6632=CARTESIAN_POINT('Origin',(183.481502506493,-22.9619250064101,55.9975995945293));
#6633=CARTESIAN_POINT('',(158.47224362268,-22.9619250064101,55.7660318462753));
#6634=CARTESIAN_POINT('',(183.481502506493,-22.9619250064101,55.9975995945293));
#6635=CARTESIAN_POINT('',(158.47224362268,-11.480962503205,55.7660318462753));
#6636=CARTESIAN_POINT('Origin',(183.425949203617,-22.9619250064101,61.9973424082289));
#6637=CARTESIAN_POINT('',(158.47224362268,-17.0993058558373,60.4896385760844));
#6638=CARTESIAN_POINT('',(183.437769055293,-17.0993058558373,60.7208013840375));
#6639=CARTESIAN_POINT('Origin',(158.47224362268,-22.9619250064101,61.7662890436003));
#6640=CARTESIAN_POINT('Origin',(183.47224362268,0.,56.9975567301459));
#6641=CARTESIAN_POINT('',(158.47224362268,17.0993058558373,60.4896385760844));
#6642=CARTESIAN_POINT('',(183.437769055293,17.0993058558373,60.7208013840375));
#6643=CARTESIAN_POINT('Origin',(158.47224362268,0.,56.7660747124961));
#6644=CARTESIAN_POINT('Origin',(183.425949203617,22.9619250064101,61.9973424082289));
#6645=CARTESIAN_POINT('',(158.47224362268,22.9619250064101,55.7660318462753));
#6646=CARTESIAN_POINT('',(183.481502506493,22.9619250064101,55.9975995945293));
#6647=CARTESIAN_POINT('Origin',(158.47224362268,22.9619250064101,61.7662890436003));
#6648=CARTESIAN_POINT('Origin',(183.481502506493,35.,55.9975995945293));
#6649=CARTESIAN_POINT('',(158.47224362268,32.,55.7660318462753));
#6650=CARTESIAN_POINT('',(137.675244927441,32.,55.573466597514));
#6651=CARTESIAN_POINT('',(158.47224362268,17.5,55.7660318462753));
#6652=CARTESIAN_POINT('Origin',(137.703021578879,32.,52.5735951906642));
#6653=CARTESIAN_POINT('Origin',(158.47224362268,32.,52.7659032476128));
#6654=CARTESIAN_POINT('Origin',(158.47224362268,0.,37.));
#6655=CARTESIAN_POINT('',(158.47224362268,0.,37.));
#6656=CARTESIAN_POINT('',(158.47224362268,-9.5,56.9975567301459));
#6657=CARTESIAN_POINT('Origin',(158.47224362268,0.,56.9975567301459));
#6658=CARTESIAN_POINT('Origin',(183.47224362268,0.,56.9975567301459));
#6659=CARTESIAN_POINT('',(183.47224362268,9.5,56.9975567301459));
#6660=CARTESIAN_POINT('',(183.47224362268,-9.5,56.9975567301459));
#6661=CARTESIAN_POINT('Origin',(183.47224362268,0.,56.9975567301459));
#6662=CARTESIAN_POINT('Origin',(183.47224362268,0.,56.9975567301459));
#6663=CARTESIAN_POINT('',(183.47224362268,-9.5,56.9975567301459));
#6664=CARTESIAN_POINT('Origin',(183.47224362268,0.,74.9975567301459));
#6665=CARTESIAN_POINT('',(183.47224362268,0.,56.9975567301459));
#6666=CARTESIAN_POINT('',(183.47224362268,0.,56.9975567301459));
#6667=CARTESIAN_POINT('Origin',(125.145502758917,38.,0.));
#6668=CARTESIAN_POINT('Origin',(125.145502758917,38.,0.));
#6669=CARTESIAN_POINT('Origin',(124.,38.,11.));
#6670=CARTESIAN_POINT('',(124.,38.,8.));
#6671=CARTESIAN_POINT('Origin',(156.,49.,8.));
#6672=CARTESIAN_POINT('',(152.,50.,8.));
#6673=CARTESIAN_POINT('Origin',(156.,50.,8.));
#6674=CARTESIAN_POINT('Origin',(60.,-38.,11.));
#6675=CARTESIAN_POINT('Origin',(28.,50.,0.));
#6676=CARTESIAN_POINT('',(24.,50.,0.));
#6677=CARTESIAN_POINT('',(24.,50.,0.));
#6678=CARTESIAN_POINT('Origin',(28.,50.,0.));
#6679=CARTESIAN_POINT('Origin',(28.,35.,0.));
#6680=CARTESIAN_POINT('Origin',(28.,35.,0.));
#6681=CARTESIAN_POINT('Origin',(28.,-50.,0.));
#6682=CARTESIAN_POINT('',(24.,-50.,0.));
#6683=CARTESIAN_POINT('Origin',(156.,50.,0.));
#6684=CARTESIAN_POINT('',(152.,50.,0.));
#6685=CARTESIAN_POINT('',(152.,50.,0.));
#6686=CARTESIAN_POINT('Origin',(156.,50.,0.));
#6687=CARTESIAN_POINT('Origin',(156.,-50.,0.));
#6688=CARTESIAN_POINT('',(152.,-50.,0.));
#6689=CARTESIAN_POINT('Origin',(184.,-35.,0.));
#6690=CARTESIAN_POINT('',(184.,-35.,0.));
#6691=CARTESIAN_POINT('Origin',(10.8741674113267,19.,62.));
#6692=CARTESIAN_POINT('',(13.47224362268,16.,62.));
#6693=CARTESIAN_POINT('Origin',(13.47224362268,19.,62.));
#6694=CARTESIAN_POINT('',(8.27609119997336,19.,62.));
#6695=CARTESIAN_POINT('',(10.8741674113267,17.5,62.));
#6696=CARTESIAN_POINT('Origin',(22.47224362268,19.,62.));
#6697=CARTESIAN_POINT('',(22.47224362268,16.,62.));
#6698=CARTESIAN_POINT('Origin',(10.8741674113267,-19.,62.));
#6699=CARTESIAN_POINT('',(13.47224362268,-22.,62.));
#6700=CARTESIAN_POINT('Origin',(13.47224362268,-19.,62.));
#6701=CARTESIAN_POINT('',(8.27609119997336,-19.,62.));
#6702=CARTESIAN_POINT('',(10.8741674113267,-20.5,62.));
#6703=CARTESIAN_POINT('Origin',(22.47224362268,-19.,62.));
#6704=CARTESIAN_POINT('',(22.47224362268,-22.,62.));
#6705=CARTESIAN_POINT('Origin',(31.47224362268,0.,37.));
#6706=CARTESIAN_POINT('Origin',(16.97224362268,0.,82.));
#6707=CARTESIAN_POINT('',(16.97224362268,0.,82.));
#6708=CARTESIAN_POINT('Origin',(35.,0.,52.));
#6709=CARTESIAN_POINT('Origin',(184.,0.,0.));
#6710=CARTESIAN_POINT('',(184.,0.,0.));
#6711=CARTESIAN_POINT('Origin',(183.47224362268,0.,56.9975567301459));
#6712=CARTESIAN_POINT('',(0.,0.,0.));
#6713=CARTESIAN_POINT('Origin',(-40.,19.,55.));
#6714=CARTESIAN_POINT('',(-40.,22.,55.));
#6715=CARTESIAN_POINT('Origin',(-40.,19.,55.));
#6716=CARTESIAN_POINT('',(-22.,22.,55.));
#6717=CARTESIAN_POINT('',(-40.,22.,55.));
#6718=CARTESIAN_POINT('Origin',(-22.,19.,55.));
#6719=CARTESIAN_POINT('Origin',(-22.,19.,55.));
#6720=CARTESIAN_POINT('Origin',(-40.,-19.0000002831221,55.));
#6721=CARTESIAN_POINT('',(-40.,-16.0000002831221,55.));
#6722=CARTESIAN_POINT('Origin',(-40.,-19.0000002831221,55.));
#6723=CARTESIAN_POINT('',(-22.,-16.0000002831221,55.));
#6724=CARTESIAN_POINT('',(-40.,-16.0000002831221,55.));
#6725=CARTESIAN_POINT('Origin',(-22.,-19.0000002831221,55.));
#6726=CARTESIAN_POINT('Origin',(-22.,-19.0000002831221,55.));
#6727=CARTESIAN_POINT('Ctrl Pts',(-6.37867965644035,34.9999541371497,51.0165890496372));
#6728=CARTESIAN_POINT('Ctrl Pts',(-6.37867965644035,34.9950012836112,51.9122953199069));
#6729=CARTESIAN_POINT('Ctrl Pts',(-6.37867965644035,34.2384990747876,53.4551378138109));
#6730=CARTESIAN_POINT('Ctrl Pts',(-6.37867965644035,32.6710924757466,54.000000684689));
#6731=CARTESIAN_POINT('Ctrl Pts',(-6.37867965644035,31.999999845455,54.0000006501177));
#6732=CARTESIAN_POINT('Ctrl Pts',(-6.66439394215464,34.9999541371497,51.0165890496372));
#6733=CARTESIAN_POINT('Ctrl Pts',(-6.66439394215464,34.9950007331352,51.9123948715632));
#6734=CARTESIAN_POINT('Ctrl Pts',(-6.66439394215464,34.2386138683966,53.4551824004139));
#6735=CARTESIAN_POINT('Ctrl Pts',(-6.66439394215464,32.6711670631254,54.0000006846929));
#6736=CARTESIAN_POINT('Ctrl Pts',(-6.66439394215464,31.999999845455,54.0000006501177));
#6737=CARTESIAN_POINT('Ctrl Pts',(-7.29086286479755,35.1192315079769,51.0172485999472));
#6738=CARTESIAN_POINT('Ctrl Pts',(-7.29086286479755,35.1140827400347,51.9483853061338));
#6739=CARTESIAN_POINT('Ctrl Pts',(-7.29086286479755,34.3272906341022,53.5526716241217));
#6740=CARTESIAN_POINT('Ctrl Pts',(-7.29086286479755,32.6976381187965,54.1192798803784));
#6741=CARTESIAN_POINT('Ctrl Pts',(-7.29086286479755,31.9999998393103,54.1192798444396));
#6742=CARTESIAN_POINT('Ctrl Pts',(-8.04466290756678,35.7074899498764,51.0205014050265));
#6743=CARTESIAN_POINT('Ctrl Pts',(-8.04466290756678,35.7013690886002,52.1274377967375));
#6744=CARTESIAN_POINT('Ctrl Pts',(-8.04466290756678,34.7664221252725,54.0341696623003));
#6745=CARTESIAN_POINT('Ctrl Pts',(-8.04466290756678,32.8293530013812,54.7075473222703));
#6746=CARTESIAN_POINT('Ctrl Pts',(-8.04466290756678,31.9999998090057,54.7075472795461));
#6747=CARTESIAN_POINT('Ctrl Pts',(-8.43400626930132,36.4500762616906,51.0246075739394));
#6748=CARTESIAN_POINT('Ctrl Pts',(-8.43400626930132,36.4427288681681,52.3533580401398));
#6749=CARTESIAN_POINT('Ctrl Pts',(-8.43400626930133,35.3206360783581,54.6419397551437));
#6750=CARTESIAN_POINT('Ctrl Pts',(-8.43400626930132,32.9955433713278,55.4501449951943));
#6751=CARTESIAN_POINT('Ctrl Pts',(-8.43400626930132,31.9999997707508,55.4501449439089));
#6752=CARTESIAN_POINT('Ctrl Pts',(-8.5,36.906959612409,51.0271339337466));
#6753=CARTESIAN_POINT('Ctrl Pts',(-8.5,36.8988586235225,52.4921694904538));
#6754=CARTESIAN_POINT('Ctrl Pts',(-8.5,35.6614045759983,55.0157918682276));
#6755=CARTESIAN_POINT('Ctrl Pts',(-8.5,33.0976526250101,55.9070353359372));
#6756=CARTESIAN_POINT('Ctrl Pts',(-8.5,31.9999997472141,55.9070352793916));
#6757=CARTESIAN_POINT('Ctrl Pts',(-8.5,37.1212420507768,51.0283188194265));
#6758=CARTESIAN_POINT('Ctrl Pts',(-8.5,37.1127870009151,52.5573850673551));
#6759=CARTESIAN_POINT('Ctrl Pts',(-8.5,35.8213569502497,55.1911819510015));
#6760=CARTESIAN_POINT('Ctrl Pts',(-8.5,33.1456265161503,56.1213210526943));
#6761=CARTESIAN_POINT('Ctrl Pts',(-8.5,31.9999997361752,56.1213209936773));
#6762=CARTESIAN_POINT('',(-8.5,31.9999997361752,56.1213209936773));
#6763=CARTESIAN_POINT('',(-6.37867965644035,31.999999845455,54.0000006501177));
#6764=CARTESIAN_POINT('Ctrl Pts',(-8.5,31.9999997361752,56.1213209936773));
#6765=CARTESIAN_POINT('Ctrl Pts',(-8.5,31.9999997472141,55.9070352793916));
#6766=CARTESIAN_POINT('Ctrl Pts',(-8.43400626930132,31.9999997707508,55.4501449439089));
#6767=CARTESIAN_POINT('Ctrl Pts',(-8.04466290756678,31.9999998090057,54.7075472795461));
#6768=CARTESIAN_POINT('Ctrl Pts',(-7.29086286479755,31.9999998393103,54.1192798444396));
#6769=CARTESIAN_POINT('Ctrl Pts',(-6.66439394215464,31.999999845455,54.0000006501177));
#6770=CARTESIAN_POINT('Ctrl Pts',(-6.37867965644035,31.999999845455,54.0000006501177));
#6771=CARTESIAN_POINT('',(-6.37867965644035,34.9999541371497,51.0165890496372));
#6772=CARTESIAN_POINT('Ctrl Pts',(-6.37867965644035,31.999999845455,54.0000006501177));
#6773=CARTESIAN_POINT('Ctrl Pts',(-6.37867965644035,32.6710924757466,54.000000684689));
#6774=CARTESIAN_POINT('Ctrl Pts',(-6.37867965644035,34.2384990747876,53.4551378138109));
#6775=CARTESIAN_POINT('Ctrl Pts',(-6.37867965644035,34.9950012836112,51.9122953199069));
#6776=CARTESIAN_POINT('Ctrl Pts',(-6.37867965644035,34.9999541371497,51.0165890496372));
#6777=CARTESIAN_POINT('',(-8.5,34.9999446647671,55.1506938537381));
#6778=CARTESIAN_POINT('Ctrl Pts',(-6.37867965644035,34.9999541371497,51.0165890496373));
#6779=CARTESIAN_POINT('Ctrl Pts',(-6.38025523414058,34.9999541371497,51.0165890496373));
#6780=CARTESIAN_POINT('Ctrl Pts',(-6.38176387508139,34.9999541364188,51.0169080380021));
#6781=CARTESIAN_POINT('Ctrl Pts',(-6.3850668587029,34.9999541336229,51.0181283084381));
#6782=CARTESIAN_POINT('Ctrl Pts',(-6.38702023223131,34.9999541311292,51.0192166501386));
#6783=CARTESIAN_POINT('Ctrl Pts',(-6.39241151026715,34.9999541222732,51.0230818054667));
#6784=CARTESIAN_POINT('Ctrl Pts',(-6.39586971593905,34.9999541150669,51.0262269686459));
#6785=CARTESIAN_POINT('Ctrl Pts',(-6.4053209430701,34.9999540937118,51.0355472789196));
#6786=CARTESIAN_POINT('Ctrl Pts',(-6.4125881509423,34.9999540754092,51.0435353194066));
#6787=CARTESIAN_POINT('Ctrl Pts',(-6.43129945172038,34.9999540271935,51.0645787901438));
#6788=CARTESIAN_POINT('Ctrl Pts',(-6.44799684949083,34.9999539825086,51.0840813028394));
#6789=CARTESIAN_POINT('Ctrl Pts',(-6.48257634326567,34.9999538896126,51.1246252399336));
#6790=CARTESIAN_POINT('Ctrl Pts',(-6.51348072849312,34.9999538056414,51.161273784187));
#6791=CARTESIAN_POINT('Ctrl Pts',(-6.58721417125074,34.9999536047906,51.2489339939019));
#6792=CARTESIAN_POINT('Ctrl Pts',(-6.64388575517693,34.9999534494532,51.3167302659389));
#6793=CARTESIAN_POINT('Ctrl Pts',(-6.8042901846373,34.9999530064479,51.5100775053381));
#6794=CARTESIAN_POINT('Ctrl Pts',(-6.91298478299303,34.9999527015254,51.6431593731394));
#6795=CARTESIAN_POINT('Ctrl Pts',(-7.23837215274935,34.9999517601401,52.0540217934736));
#6796=CARTESIAN_POINT('Ctrl Pts',(-7.4499833285231,34.9999511070469,52.3390607643293));
#6797=CARTESIAN_POINT('Ctrl Pts',(-7.96154279702925,34.9999492924801,53.1310184777057));
#6798=CARTESIAN_POINT('Ctrl Pts',(-8.30443682747778,34.9999478076447,53.7790667327638));
#6799=CARTESIAN_POINT('Ctrl Pts',(-8.47893057631952,34.9999456402076,54.7250327436578));
#6800=CARTESIAN_POINT('Ctrl Pts',(-8.5,34.9999451531404,54.9376105145217));
#6801=CARTESIAN_POINT('Ctrl Pts',(-8.5,34.9999446649149,55.1506938535244));
#6802=CARTESIAN_POINT('Ctrl Pts',(-8.5,35.0003235118796,55.1512179007789));
#6803=CARTESIAN_POINT('Ctrl Pts',(-8.5,34.1372307533344,55.7747966654739));
#6804=CARTESIAN_POINT('Ctrl Pts',(-8.5,33.0681306896806,56.1213210487021));
#6805=CARTESIAN_POINT('Ctrl Pts',(-8.5,31.9999997361752,56.1213209936773));
#6806=CARTESIAN_POINT('Ctrl Pts',(-6.37867965644035,31.999999845455,54.0000006501177));
#6807=CARTESIAN_POINT('Ctrl Pts',(-6.37867965644035,27.7891836451619,54.0000004331975));
#6808=CARTESIAN_POINT('Ctrl Pts',(-6.37867965644035,23.5940884943755,54.0000002170871));
#6809=CARTESIAN_POINT('Ctrl Pts',(-6.37867965644035,19.3800314873921,54.));
#6810=CARTESIAN_POINT('Ctrl Pts',(-6.66439394215464,31.999999845455,54.0000006501177));
#6811=CARTESIAN_POINT('Ctrl Pts',(-6.66439394215464,27.7891836451619,54.0000004331975));
#6812=CARTESIAN_POINT('Ctrl Pts',(-6.66439394215464,23.5940884943755,54.0000002170871));
#6813=CARTESIAN_POINT('Ctrl Pts',(-6.66439394215464,19.3800314873921,54.));
#6814=CARTESIAN_POINT('Ctrl Pts',(-7.29086126549403,31.9999998393104,54.1192791631438));
#6815=CARTESIAN_POINT('Ctrl Pts',(-7.29086126549403,27.7891836390173,54.1192789462237));
#6816=CARTESIAN_POINT('Ctrl Pts',(-7.29086126549403,23.5940884882309,54.1192787301133));
#6817=CARTESIAN_POINT('Ctrl Pts',(-7.29086126549403,19.3800314812474,54.1192785130262));
#6818=CARTESIAN_POINT('Ctrl Pts',(-8.04466232388412,31.9999998090057,54.7075471088815));
#6819=CARTESIAN_POINT('Ctrl Pts',(-8.04466232388412,27.7891836087127,54.7075468919613));
#6820=CARTESIAN_POINT('Ctrl Pts',(-8.04466232388412,23.5940884579263,54.707546675851));
#6821=CARTESIAN_POINT('Ctrl Pts',(-8.04466232388412,19.3800314509428,54.7075464587638));
#6822=CARTESIAN_POINT('Ctrl Pts',(-8.43400552734115,31.9999997707508,55.4501449226738));
#6823=CARTESIAN_POINT('Ctrl Pts',(-8.43400552734115,27.7891835704577,55.4501447057536));
#6824=CARTESIAN_POINT('Ctrl Pts',(-8.43400552734115,23.5940884196713,55.4501444896432));
#6825=CARTESIAN_POINT('Ctrl Pts',(-8.43400552734115,19.3800314126879,55.4501442725561));
#6826=CARTESIAN_POINT('Ctrl Pts',(-8.5,31.9999997472141,55.9070352793916));
#6827=CARTESIAN_POINT('Ctrl Pts',(-8.5,27.789183546921,55.9070350624714));
#6828=CARTESIAN_POINT('Ctrl Pts',(-8.5,23.5940883961346,55.9070348463611));
#6829=CARTESIAN_POINT('Ctrl Pts',(-8.5,19.3800313891512,55.9070346292739));
#6830=CARTESIAN_POINT('Ctrl Pts',(-8.5,31.9999997361752,56.1213209936773));
#6831=CARTESIAN_POINT('Ctrl Pts',(-8.5,27.7891835358821,56.1213207767571));
#6832=CARTESIAN_POINT('Ctrl Pts',(-8.5,23.5940883850957,56.1213205606468));
#6833=CARTESIAN_POINT('Ctrl Pts',(-8.5,19.3800313781122,56.1213203435596));
#6834=CARTESIAN_POINT('',(-8.5,19.3800313781122,56.1213203435596));
#6835=CARTESIAN_POINT('',(-6.37867965644035,19.3800314873921,54.));
#6836=CARTESIAN_POINT('Ctrl Pts',(-8.5,19.3800313781122,56.1213203435596));
#6837=CARTESIAN_POINT('Ctrl Pts',(-8.5,19.3800313891512,55.9070346292739));
#6838=CARTESIAN_POINT('Ctrl Pts',(-8.43400552734115,19.3800314126879,55.4501442725561));
#6839=CARTESIAN_POINT('Ctrl Pts',(-8.04466232388412,19.3800314509428,54.7075464587638));
#6840=CARTESIAN_POINT('Ctrl Pts',(-7.29086126549403,19.3800314812474,54.1192785130262));
#6841=CARTESIAN_POINT('Ctrl Pts',(-6.66439394215464,19.3800314873921,54.));
#6842=CARTESIAN_POINT('Ctrl Pts',(-6.37867965644035,19.3800314873921,54.));
#6843=CARTESIAN_POINT('Ctrl Pts',(-6.37867965644035,19.3800314873921,54.));
#6844=CARTESIAN_POINT('Ctrl Pts',(-6.37867965644035,23.5940884943755,54.0000002170871));
#6845=CARTESIAN_POINT('Ctrl Pts',(-6.37867965644035,27.7891836451619,54.0000004331975));
#6846=CARTESIAN_POINT('Ctrl Pts',(-6.37867965644035,31.999999845455,54.0000006501177));
#6847=CARTESIAN_POINT('Ctrl Pts',(-8.5,31.9999997361752,56.1213209936773));
#6848=CARTESIAN_POINT('Ctrl Pts',(-8.5,27.7891835358821,56.1213207767571));
#6849=CARTESIAN_POINT('Ctrl Pts',(-8.5,23.5940883850957,56.1213205606468));
#6850=CARTESIAN_POINT('Ctrl Pts',(-8.5,19.3800313781122,56.1213203435596));
#6851=CARTESIAN_POINT('Ctrl Pts',(-6.37867965644035,19.3800304312095,54.0000000000003));
#6852=CARTESIAN_POINT('Ctrl Pts',(-6.37867965644035,18.9297963927261,54.00000021257));
#6853=CARTESIAN_POINT('Ctrl Pts',(-6.37867965644035,17.9034130389181,54.3199295949321));
#6854=CARTESIAN_POINT('Ctrl Pts',(-6.37867965644035,17.2949884311804,55.2350357080536));
#6855=CARTESIAN_POINT('Ctrl Pts',(-6.37867965644035,17.1834464391566,55.8134832037259));
#6856=CARTESIAN_POINT('Ctrl Pts',(-6.66439394215464,19.3800304312095,54.0000000000003));
#6857=CARTESIAN_POINT('Ctrl Pts',(-6.66439394215464,18.9298634995458,54.0000002125383));
#6858=CARTESIAN_POINT('Ctrl Pts',(-6.66439394215464,17.9035184186743,54.3199764064705));
#6859=CARTESIAN_POINT('Ctrl Pts',(-6.66439394215464,17.2949718059861,55.2351219249287));
#6860=CARTESIAN_POINT('Ctrl Pts',(-6.66439394215464,17.1834464391566,55.8134832037259));
#6861=CARTESIAN_POINT('Ctrl Pts',(-7.29085029793421,19.3800304875225,54.1192738233668));
#6862=CARTESIAN_POINT('Ctrl Pts',(-7.29085029793421,18.9536797671411,54.1192740246605));
#6863=CARTESIAN_POINT('Ctrl Pts',(-7.29085029793421,17.9819509665207,54.4220604781489));
#6864=CARTESIAN_POINT('Ctrl Pts',(-7.29085029793421,17.4061878303299,55.2883038245807));
#6865=CARTESIAN_POINT('Ctrl Pts',(-7.29085029793421,17.3005627451802,55.8360667332079));
#6866=CARTESIAN_POINT('Ctrl Pts',(-8.04465837989031,19.3800307652641,54.7075453005511));
#6867=CARTESIAN_POINT('Ctrl Pts',(-8.04465837989031,19.0721849320778,54.7075454458949));
#6868=CARTESIAN_POINT('Ctrl Pts',(-8.04465837989031,18.3704231339243,54.9262762166006));
#6869=CARTESIAN_POINT('Ctrl Pts',(-8.04465837989031,17.9544595302371,55.5519398552372));
#6870=CARTESIAN_POINT('Ctrl Pts',(-8.04465837989031,17.8781931120305,55.9474511583354));
#6871=CARTESIAN_POINT('Ctrl Pts',(-8.43400047932409,19.3800311158686,55.4501441545312));
#6872=CARTESIAN_POINT('Ctrl Pts',(-8.43400047932409,19.221708029536,55.4501442292806));
#6873=CARTESIAN_POINT('Ctrl Pts',(-8.43400047932409,18.8606961296434,55.5627187553402));
#6874=CARTESIAN_POINT('Ctrl Pts',(-8.43400047932409,18.6465825795345,55.8846473578588));
#6875=CARTESIAN_POINT('Ctrl Pts',(-8.43400047932409,18.6073592624962,56.0880562185142));
#6876=CARTESIAN_POINT('Ctrl Pts',(-8.5,19.3800313315811,55.907034629274));
#6877=CARTESIAN_POINT('Ctrl Pts',(-8.5,19.3135767217403,55.9070346606493));
#6878=CARTESIAN_POINT('Ctrl Pts',(-8.5,19.1621419276791,55.9542072360834));
#6879=CARTESIAN_POINT('Ctrl Pts',(-8.5,19.0724487625994,56.0891857833112));
#6880=CARTESIAN_POINT('Ctrl Pts',(-8.5,19.055985148285,56.1745647181597));
#6881=CARTESIAN_POINT('Ctrl Pts',(-8.5,19.3800314327522,56.1213203435597));
#6882=CARTESIAN_POINT('Ctrl Pts',(-8.5,19.3567392996677,56.1213203545566));
#6883=CARTESIAN_POINT('Ctrl Pts',(-8.5,19.3036410093805,56.1378713860528));
#6884=CARTESIAN_POINT('Ctrl Pts',(-8.5,19.2721651418894,56.1852129274543));
#6885=CARTESIAN_POINT('Ctrl Pts',(-8.5,19.2663946965196,56.2151379773172));
#6886=CARTESIAN_POINT('',(-8.5,19.2663946965196,56.2151379773172));
#6887=CARTESIAN_POINT('',(-6.37867965644035,17.1834464391566,55.8134832037257));
#6888=CARTESIAN_POINT('Ctrl Pts',(-8.5,19.2663946965196,56.2151379773172));
#6889=CARTESIAN_POINT('Ctrl Pts',(-8.5,19.055985148285,56.1745647181597));
#6890=CARTESIAN_POINT('Ctrl Pts',(-8.43400047932409,18.6073592624962,56.0880562185142));
#6891=CARTESIAN_POINT('Ctrl Pts',(-8.04465837989031,17.8781931120305,55.9474511583354));
#6892=CARTESIAN_POINT('Ctrl Pts',(-7.29085029793421,17.3005627451802,55.8360667332079));
#6893=CARTESIAN_POINT('Ctrl Pts',(-6.66439394215464,17.1834464391566,55.8134832037259));
#6894=CARTESIAN_POINT('Ctrl Pts',(-6.37867965644035,17.1834464391566,55.8134832037259));
#6895=CARTESIAN_POINT('Ctrl Pts',(-6.37867965644035,17.1834464391566,55.8134832037259));
#6896=CARTESIAN_POINT('Ctrl Pts',(-6.37867965644035,17.2949884311804,55.2350357080536));
#6897=CARTESIAN_POINT('Ctrl Pts',(-6.37867965644035,17.9034130389181,54.3199295949321));
#6898=CARTESIAN_POINT('Ctrl Pts',(-6.37867965644035,18.9297963927261,54.00000021257));
#6899=CARTESIAN_POINT('Ctrl Pts',(-6.37867965644035,19.3800304312095,54.0000000000003));
#6900=CARTESIAN_POINT('Ctrl Pts',(-8.5,19.3800313781122,56.1213203435597));
#6901=CARTESIAN_POINT('Ctrl Pts',(-8.5,19.3567392640789,56.1213203656498));
#6902=CARTESIAN_POINT('Ctrl Pts',(-8.5,19.3036409988323,56.137871401918));
#6903=CARTESIAN_POINT('Ctrl Pts',(-8.5,19.2721651418894,56.1852129274543));
#6904=CARTESIAN_POINT('Ctrl Pts',(-8.5,19.2663946965196,56.2151379773172));
#6905=CARTESIAN_POINT('Ctrl Pts',(-6.37867965644035,17.1834464391567,55.8134832037256));
#6906=CARTESIAN_POINT('Ctrl Pts',(-6.37867965644035,17.1179077550972,56.1533613695715));
#6907=CARTESIAN_POINT('Ctrl Pts',(-6.37867965644035,17.0393555263014,56.5042886864595));
#6908=CARTESIAN_POINT('Ctrl Pts',(-6.37867965644035,16.9519317108386,56.8453440034822));
#6909=CARTESIAN_POINT('Ctrl Pts',(-6.66439394215464,17.1834464391567,55.8134832037256));
#6910=CARTESIAN_POINT('Ctrl Pts',(-6.66439394215464,17.1179065063808,56.1533678453107));
#6911=CARTESIAN_POINT('Ctrl Pts',(-6.66439394215464,17.0393571919978,56.5042821882919));
#6912=CARTESIAN_POINT('Ctrl Pts',(-6.66439394215464,16.9519317108386,56.8453440034822));
#6913=CARTESIAN_POINT('Ctrl Pts',(-7.2908511525663,17.3005631050862,55.8360668026084));
#6914=CARTESIAN_POINT('Ctrl Pts',(-7.2908511525663,17.2345800028592,56.1782496841166));
#6915=CARTESIAN_POINT('Ctrl Pts',(-7.2908511525663,17.1554870860676,56.531592408039));
#6916=CARTESIAN_POINT('Ctrl Pts',(-7.2908511525663,17.0674704492441,56.8749604229925));
#6917=CARTESIAN_POINT('Ctrl Pts',(-8.04465868351329,17.8781931999001,55.9474511752792));
#6918=CARTESIAN_POINT('Ctrl Pts',(-8.04465868351329,17.810004971711,56.3010696566657));
#6919=CARTESIAN_POINT('Ctrl Pts',(-8.04465868351329,17.7282761750909,56.6661880879725));
#6920=CARTESIAN_POINT('Ctrl Pts',(-8.04465868351329,17.6373180613679,57.0210313094374));
#6921=CARTESIAN_POINT('Ctrl Pts',(-8.43400087015911,18.6073592698178,56.088056219926));
#6922=CARTESIAN_POINT('Ctrl Pts',(-8.43400087015911,18.5363887387313,56.4561034927842));
#6923=CARTESIAN_POINT('Ctrl Pts',(-8.43400087015911,18.4513294878821,56.8361005713277));
#6924=CARTESIAN_POINT('Ctrl Pts',(-8.43400087015911,18.3566599854035,57.2054225576683));
#6925=CARTESIAN_POINT('Ctrl Pts',(-8.5,19.055985148285,56.1745647181597));
#6926=CARTESIAN_POINT('Ctrl Pts',(-8.5,18.9833051386494,56.551477204626));
#6927=CARTESIAN_POINT('Ctrl Pts',(-8.5,18.8961912931089,56.9406530010384));
#6928=CARTESIAN_POINT('Ctrl Pts',(-8.5,18.7992414711618,57.3188709052149));
#6929=CARTESIAN_POINT('Ctrl Pts',(-8.5,19.2663946965195,56.2151379773172));
#6930=CARTESIAN_POINT('Ctrl Pts',(-8.5,19.1929115242437,56.5962155984512));
#6931=CARTESIAN_POINT('Ctrl Pts',(-8.5,19.1048373273922,56.989681729992));
#6932=CARTESIAN_POINT('Ctrl Pts',(-8.5,19.0068161451721,57.3720791945735));
#6933=CARTESIAN_POINT('',(-8.5,19.0068161428526,57.3720791939789));
#6934=CARTESIAN_POINT('',(-6.37867965644035,16.9519317108386,56.8453440034822));
#6935=CARTESIAN_POINT('Ctrl Pts',(-8.5,19.0068161451721,57.3720791945735));
#6936=CARTESIAN_POINT('Ctrl Pts',(-8.5,18.7992414711618,57.3188709052149));
#6937=CARTESIAN_POINT('Ctrl Pts',(-8.43400087015911,18.3566599854035,57.2054225576683));
#6938=CARTESIAN_POINT('Ctrl Pts',(-8.04465868351329,17.6373180613679,57.0210313094374));
#6939=CARTESIAN_POINT('Ctrl Pts',(-7.2908511525663,17.0674704492441,56.8749604229925));
#6940=CARTESIAN_POINT('Ctrl Pts',(-6.66439394215464,16.9519317108386,56.8453440034822));
#6941=CARTESIAN_POINT('Ctrl Pts',(-6.37867965644035,16.9519317108386,56.8453440034822));
#6942=CARTESIAN_POINT('Ctrl Pts',(-6.37867965644035,16.9519317108386,56.8453440034822));
#6943=CARTESIAN_POINT('Ctrl Pts',(-6.37867965644035,17.0393555263014,56.5042886864595));
#6944=CARTESIAN_POINT('Ctrl Pts',(-6.37867965644035,17.1179077550972,56.1533613695715));
#6945=CARTESIAN_POINT('Ctrl Pts',(-6.37867965644035,17.1834464391567,55.8134832037256));
#6946=CARTESIAN_POINT('Ctrl Pts',(-8.5,19.2663946965195,56.2151379773172));
#6947=CARTESIAN_POINT('Ctrl Pts',(-8.5,19.1929115242437,56.5962155984512));
#6948=CARTESIAN_POINT('Ctrl Pts',(-8.5,19.1048373273922,56.989681729992));
#6949=CARTESIAN_POINT('Ctrl Pts',(-8.5,19.0068161451721,57.3720791945735));
#6950=CARTESIAN_POINT('Ctrl Pts',(-6.37867965629528,16.9519317107165,56.8453440039586));
#6951=CARTESIAN_POINT('Ctrl Pts',(-6.34395902543105,16.3625204948522,59.144738373737));
#6952=CARTESIAN_POINT('Ctrl Pts',(-7.21813179282277,14.2180407656508,63.4520143249812));
#6953=CARTESIAN_POINT('Ctrl Pts',(-9.58480819189232,9.76913766486894,67.3440245597847));
#6954=CARTESIAN_POINT('Ctrl Pts',(-11.1910106295689,5.89018091675158,69.0834726889151));
#6955=CARTESIAN_POINT('Ctrl Pts',(-11.9050643746374,3.17270779483425,69.7523377363836));
#6956=CARTESIAN_POINT('Ctrl Pts',(-12.3068239762497,0.360377317317033,70.0979661217499));
#6957=CARTESIAN_POINT('Ctrl Pts',(-11.9786204675957,-3.91310591747159,69.8333384317106));
#6958=CARTESIAN_POINT('Ctrl Pts',(-9.87906744362539,-9.2039373346128,67.8305030724374));
#6959=CARTESIAN_POINT('Ctrl Pts',(-7.21891300399149,-14.2217863750276,63.4517614180996));
#6960=CARTESIAN_POINT('Ctrl Pts',(-6.34395902430692,-16.3625204986098,59.1447383644959));
#6961=CARTESIAN_POINT('Ctrl Pts',(-6.37867965644035,-16.9519317131792,56.8453439943512));
#6962=CARTESIAN_POINT('Ctrl Pts',(-6.66439394200957,16.9519317107543,56.8453440038109));
#6963=CARTESIAN_POINT('Ctrl Pts',(-6.62986367742403,16.3714433629399,59.1096805950205));
#6964=CARTESIAN_POINT('Ctrl Pts',(-7.48958295564451,14.2715353296098,63.3702716486415));
#6965=CARTESIAN_POINT('Ctrl Pts',(-9.84565213340604,9.86818195374051,67.2799680929364));
#6966=CARTESIAN_POINT('Ctrl Pts',(-11.4608448228196,5.9819769902233,69.0529723976167));
#6967=CARTESIAN_POINT('Ctrl Pts',(-12.1847303919658,3.23320277617613,69.7424124829677));
#6968=CARTESIAN_POINT('Ctrl Pts',(-12.5957628559963,0.369524021153959,70.1025590335402));
#6969=CARTESIAN_POINT('Ctrl Pts',(-12.2570349822639,-3.99701914926913,69.8237052527086));
#6970=CARTESIAN_POINT('Ctrl Pts',(-10.137439575499,-9.30863506754452,67.7676071711941));
#6971=CARTESIAN_POINT('Ctrl Pts',(-7.49094960148944,-14.2753080106798,63.3705284326759));
#6972=CARTESIAN_POINT('Ctrl Pts',(-6.62986367631848,-16.3714433666239,59.109680585902));
#6973=CARTESIAN_POINT('Ctrl Pts',(-6.66439394215464,-16.9519317131792,56.8453439943512));
#6974=CARTESIAN_POINT('Ctrl Pts',(-7.29085681341187,17.0674727965435,56.8749610246921));
#6975=CARTESIAN_POINT('Ctrl Pts',(-7.25359142535474,16.5011002158146,59.0765726044006));
#6976=CARTESIAN_POINT('Ctrl Pts',(-8.07001397882514,14.4728073863862,63.2637523438959));
#6977=CARTESIAN_POINT('Ctrl Pts',(-10.3873011914576,10.1189189924078,67.2196144493972));
#6978=CARTESIAN_POINT('Ctrl Pts',(-12.0137632580413,6.19168605657765,69.0537975629472));
#6979=CARTESIAN_POINT('Ctrl Pts',(-12.7544345720524,3.36676906315595,69.779846800734));
#6980=CARTESIAN_POINT('Ctrl Pts',(-13.1824675433198,0.388852912794903,70.1655117313478));
#6981=CARTESIAN_POINT('Ctrl Pts',(-12.8242733539201,-4.17885251122572,69.8615705277069));
#6982=CARTESIAN_POINT('Ctrl Pts',(-10.6715137743796,-9.56519084510394,67.7113211237085));
#6983=CARTESIAN_POINT('Ctrl Pts',(-8.07251448834307,-14.4767690396738,63.2649464971057));
#6984=CARTESIAN_POINT('Ctrl Pts',(-7.25359142431386,-16.501100219378,59.0765725954899));
#6985=CARTESIAN_POINT('Ctrl Pts',(-7.29085681356742,-17.0674727989103,56.8749610154928));
#6986=CARTESIAN_POINT('Ctrl Pts',(-8.04466071039456,17.6373186387505,57.0210314570503));
#6987=CARTESIAN_POINT('Ctrl Pts',(-8.00890511329239,17.0603716343414,59.203097681082));
#6988=CARTESIAN_POINT('Ctrl Pts',(-8.79506791017244,15.0063077361413,63.3716260613067));
#6989=CARTESIAN_POINT('Ctrl Pts',(-11.0922237167727,10.5809826490206,67.3627780794766));
#6990=CARTESIAN_POINT('Ctrl Pts',(-12.7477737887617,6.53503905510173,69.2428293068738));
#6991=CARTESIAN_POINT('Ctrl Pts',(-13.5171077521835,3.57586091281896,69.9979929341239));
#6992=CARTESIAN_POINT('Ctrl Pts',(-13.9714915825714,0.417585392783423,70.4051811242831));
#6993=CARTESIAN_POINT('Ctrl Pts',(-13.5838871253004,-4.45711569224503,70.0794076087635));
#6994=CARTESIAN_POINT('Ctrl Pts',(-11.3703804176736,-10.0175009980528,67.8568949792364));
#6995=CARTESIAN_POINT('Ctrl Pts',(-8.79918909864043,-15.0105616090737,63.3737788829551));
#6996=CARTESIAN_POINT('Ctrl Pts',(-8.00890511229057,-17.0603716379541,59.2030976722323));
#6997=CARTESIAN_POINT('Ctrl Pts',(-8.04466071054412,-17.637318641161,57.0210314479333));
#6998=CARTESIAN_POINT('Ctrl Pts',(-8.4340034697139,18.3566600404711,57.2054225712016));
#6999=CARTESIAN_POINT('Ctrl Pts',(-8.4131142502009,17.7531399341081,59.4333522781253));
#7000=CARTESIAN_POINT('Ctrl Pts',(-9.25473584961778,15.6047661069344,63.6632982361135));
#7001=CARTESIAN_POINT('Ctrl Pts',(-11.6235485907392,11.0496166725652,67.6613555550095));
#7002=CARTESIAN_POINT('Ctrl Pts',(-13.3433740013405,6.86931369540524,69.5540876559054));
#7003=CARTESIAN_POINT('Ctrl Pts',(-14.1539310599708,3.77606032687716,70.3194772832757));
#7004=CARTESIAN_POINT('Ctrl Pts',(-14.640309711713,0.444537213945822,70.7360626019776));
#7005=CARTESIAN_POINT('Ctrl Pts',(-14.2193675814448,-4.72121257881821,70.4000180814526));
#7006=CARTESIAN_POINT('Ctrl Pts',(-11.9071685821935,-10.4691197613114,68.1548863776572));
#7007=CARTESIAN_POINT('Ctrl Pts',(-9.260484524673,-15.6092803900723,63.6659970008699));
#7008=CARTESIAN_POINT('Ctrl Pts',(-8.41311424910159,-17.7531399378894,59.4333522691111));
#7009=CARTESIAN_POINT('Ctrl Pts',(-8.43400346980125,-18.3566600429926,57.205422561893));
#7010=CARTESIAN_POINT('Ctrl Pts',(-8.49999999997069,18.7992414711669,57.3188709046107));
#7011=CARTESIAN_POINT('Ctrl Pts',(-8.49299518410109,18.1792591692181,59.5977676897671));
#7012=CARTESIAN_POINT('Ctrl Pts',(-9.40272281752661,15.9716471367371,63.9019111675863));
#7013=CARTESIAN_POINT('Ctrl Pts',(-11.8654901989597,11.3347117740451,67.9082032467995));
#7014=CARTESIAN_POINT('Ctrl Pts',(-13.6485420048835,7.07174259115336,69.8004362117152));
#7015=CARTESIAN_POINT('Ctrl Pts',(-14.4941330672572,3.89706591383746,70.5665966564561));
#7016=CARTESIAN_POINT('Ctrl Pts',(-15.0053202848577,0.4607752223178,70.9850969586586));
#7017=CARTESIAN_POINT('Ctrl Pts',(-14.5597383973889,-4.8806191580855,70.6464457045767));
#7018=CARTESIAN_POINT('Ctrl Pts',(-12.1586585520426,-10.7435452304658,68.4020692991085));
#7019=CARTESIAN_POINT('Ctrl Pts',(-9.40952176374036,-15.9763233391107,63.9048466218829));
#7020=CARTESIAN_POINT('Ctrl Pts',(-8.49299518288957,-18.1792591731044,59.5977676805651));
#7021=CARTESIAN_POINT('Ctrl Pts',(-8.5,-18.7992414737574,57.3188708950889));
#7022=CARTESIAN_POINT('Ctrl Pts',(-8.5,19.0068161451757,57.3720791939752));
#7023=CARTESIAN_POINT('Ctrl Pts',(-8.5000000012708,18.3795907455684,59.6791628056302));
#7024=CARTESIAN_POINT('Ctrl Pts',(-9.44624036508731,16.1467970192983,64.026720059828));
#7025=CARTESIAN_POINT('Ctrl Pts',(-11.9649851410576,11.4734910366497,68.0424265260941));
#7026=CARTESIAN_POINT('Ctrl Pts',(-13.7856701385902,7.17121819021727,69.9345670496955));
#7027=CARTESIAN_POINT('Ctrl Pts',(-14.6514601964537,3.95675939413664,70.7007389799831));
#7028=CARTESIAN_POINT('Ctrl Pts',(-15.1765964061977,0.468832098437293,71.119759719284));
#7029=CARTESIAN_POINT('Ctrl Pts',(-14.7173999119069,-4.95944961184219,70.7802866584454));
#7030=CARTESIAN_POINT('Ctrl Pts',(-12.2640711444334,-10.8775402354315,68.5371535059029));
#7031=CARTESIAN_POINT('Ctrl Pts',(-9.45356730467222,-16.1515515068563,64.0297644640651));
#7032=CARTESIAN_POINT('Ctrl Pts',(-8.5,-18.3795907494999,59.6791627963227));
#7033=CARTESIAN_POINT('Ctrl Pts',(-8.5,-19.0068161477964,57.3720791843357));
#7034=CARTESIAN_POINT('',(-8.49999999999999,-19.0068161477964,57.3720791843357));
#7035=CARTESIAN_POINT('',(-6.37867965644035,-16.9519317131792,56.8453439943512));
#7036=CARTESIAN_POINT('Ctrl Pts',(-8.5,-19.0068161477964,57.3720791843357));
#7037=CARTESIAN_POINT('Ctrl Pts',(-8.5,-18.7992414737574,57.3188708950889));
#7038=CARTESIAN_POINT('Ctrl Pts',(-8.43400346980125,-18.3566600429926,57.205422561893));
#7039=CARTESIAN_POINT('Ctrl Pts',(-8.04466071054412,-17.637318641161,57.0210314479333));
#7040=CARTESIAN_POINT('Ctrl Pts',(-7.29085681356742,-17.0674727989103,56.8749610154928));
#7041=CARTESIAN_POINT('Ctrl Pts',(-6.66439394215464,-16.9519317131792,56.8453439943512));
#7042=CARTESIAN_POINT('Ctrl Pts',(-6.37867965644035,-16.9519317131792,56.8453439943512));
#7043=CARTESIAN_POINT('Ctrl Pts',(-6.37867965644035,-16.9519317131792,56.8453439943512));
#7044=CARTESIAN_POINT('Ctrl Pts',(-6.34395902430692,-16.3625204986098,59.1447383644959));
#7045=CARTESIAN_POINT('Ctrl Pts',(-7.21891300399149,-14.2217863750276,63.4517614180996));
#7046=CARTESIAN_POINT('Ctrl Pts',(-9.87906744362539,-9.2039373346128,67.8305030724374));
#7047=CARTESIAN_POINT('Ctrl Pts',(-11.9786204675957,-3.91310591747159,69.8333384317106));
#7048=CARTESIAN_POINT('Ctrl Pts',(-12.3068239762497,0.360377317317033,70.0979661217499));
#7049=CARTESIAN_POINT('Ctrl Pts',(-11.9050643746374,3.17270779483425,69.7523377363836));
#7050=CARTESIAN_POINT('Ctrl Pts',(-11.1910106295689,5.89018091675158,69.0834726889151));
#7051=CARTESIAN_POINT('Ctrl Pts',(-9.58480819189232,9.76913766486894,67.3440245597847));
#7052=CARTESIAN_POINT('Ctrl Pts',(-7.21813179282277,14.2180407656508,63.4520143249812));
#7053=CARTESIAN_POINT('Ctrl Pts',(-6.34395902543105,16.3625204948522,59.144738373737));
#7054=CARTESIAN_POINT('Ctrl Pts',(-6.37867965629528,16.9519317107165,56.8453440039586));
#7055=CARTESIAN_POINT('Ctrl Pts',(-8.5,19.0068161451757,57.3720791939752));
#7056=CARTESIAN_POINT('Ctrl Pts',(-8.5000000012708,18.3795907455684,59.6791628056302));
#7057=CARTESIAN_POINT('Ctrl Pts',(-9.44624036508731,16.1467970192983,64.026720059828));
#7058=CARTESIAN_POINT('Ctrl Pts',(-11.9649851410576,11.4734910366497,68.0424265260941));
#7059=CARTESIAN_POINT('Ctrl Pts',(-13.7856701385902,7.17121819021727,69.9345670496955));
#7060=CARTESIAN_POINT('Ctrl Pts',(-14.6514601964537,3.95675939413664,70.7007389799831));
#7061=CARTESIAN_POINT('Ctrl Pts',(-15.1765964061977,0.468832098437293,71.119759719284));
#7062=CARTESIAN_POINT('Ctrl Pts',(-14.7173999119069,-4.95944961184219,70.7802866584454));
#7063=CARTESIAN_POINT('Ctrl Pts',(-12.2640711444334,-10.8775402354315,68.5371535059029));
#7064=CARTESIAN_POINT('Ctrl Pts',(-9.45356730467222,-16.1515515068563,64.0297644640651));
#7065=CARTESIAN_POINT('Ctrl Pts',(-8.5,-18.3795907494999,59.6791627963227));
#7066=CARTESIAN_POINT('Ctrl Pts',(-8.5,-19.0068161477964,57.3720791843357));
#7067=CARTESIAN_POINT('Ctrl Pts',(-6.37867965644035,-16.9519317131792,56.8453439943512));
#7068=CARTESIAN_POINT('Ctrl Pts',(-6.37867965644035,-17.0393555276599,56.504288680396));
#7069=CARTESIAN_POINT('Ctrl Pts',(-6.37867965644035,-17.117907755524,56.153361367358));
#7070=CARTESIAN_POINT('Ctrl Pts',(-6.37867965644035,-17.1834464391567,55.8134832037256));
#7071=CARTESIAN_POINT('Ctrl Pts',(-6.66439394215464,-16.9519317131792,56.8453439943512));
#7072=CARTESIAN_POINT('Ctrl Pts',(-6.66439394215464,-17.0393571933563,56.5042821822285));
#7073=CARTESIAN_POINT('Ctrl Pts',(-6.66439394215464,-17.1179065068077,56.1533678430972));
#7074=CARTESIAN_POINT('Ctrl Pts',(-6.66439394215464,-17.1834464391567,55.8134832037256));
#7075=CARTESIAN_POINT('Ctrl Pts',(-7.29085115256629,-17.0674704516006,56.8749604137993));
#7076=CARTESIAN_POINT('Ctrl Pts',(-7.29085115256629,-17.1554870874354,56.5315924019341));
#7077=CARTESIAN_POINT('Ctrl Pts',(-7.29085115256629,-17.2345800032889,56.178249681888));
#7078=CARTESIAN_POINT('Ctrl Pts',(-7.29085115256629,-17.3005631050862,55.8360668026083));
#7079=CARTESIAN_POINT('Ctrl Pts',(-8.04465868351329,-17.6373180638031,57.0210312999373));
#7080=CARTESIAN_POINT('Ctrl Pts',(-8.04465868351329,-17.7282761765043,56.6661880816638));
#7081=CARTESIAN_POINT('Ctrl Pts',(-8.04465868351328,-17.8100049721551,56.3010696543627));
#7082=CARTESIAN_POINT('Ctrl Pts',(-8.04465868351328,-17.8781931999001,55.9474511752791));
#7083=CARTESIAN_POINT('Ctrl Pts',(-8.43400087015911,-18.356659987938,57.2054225477807));
#7084=CARTESIAN_POINT('Ctrl Pts',(-8.43400087015911,-18.4513294893531,56.8361005647618));
#7085=CARTESIAN_POINT('Ctrl Pts',(-8.43400087015911,-18.5363887391935,56.4561034903872));
#7086=CARTESIAN_POINT('Ctrl Pts',(-8.43400087015911,-18.6073592698178,56.0880562199259));
#7087=CARTESIAN_POINT('Ctrl Pts',(-8.5,-18.7992414737574,57.3188708950889));
#7088=CARTESIAN_POINT('Ctrl Pts',(-8.5,-18.8961912946155,56.9406529943141));
#7089=CARTESIAN_POINT('Ctrl Pts',(-8.5,-18.9833051391228,56.5514772021713));
#7090=CARTESIAN_POINT('Ctrl Pts',(-8.5,-19.055985148285,56.1745647181597));
#7091=CARTESIAN_POINT('Ctrl Pts',(-8.5,-19.0068161477963,57.3720791843357));
#7092=CARTESIAN_POINT('Ctrl Pts',(-8.5,-19.1048373289154,56.9896817231935));
#7093=CARTESIAN_POINT('Ctrl Pts',(-8.5,-19.1929115247223,56.5962155959693));
#7094=CARTESIAN_POINT('Ctrl Pts',(-8.5,-19.2663946965195,56.2151379773172));
#7095=CARTESIAN_POINT('',(-8.5,-19.2663946965195,56.2151379773172));
#7096=CARTESIAN_POINT('',(-6.37867965644035,-17.1834464391567,55.8134832037256));
#7097=CARTESIAN_POINT('Ctrl Pts',(-8.5,-19.2663946965195,56.2151379773172));
#7098=CARTESIAN_POINT('Ctrl Pts',(-8.5,-19.055985148285,56.1745647181597));
#7099=CARTESIAN_POINT('Ctrl Pts',(-8.43400087015911,-18.6073592698178,56.0880562199259));
#7100=CARTESIAN_POINT('Ctrl Pts',(-8.04465868351328,-17.8781931999001,55.9474511752791));
#7101=CARTESIAN_POINT('Ctrl Pts',(-7.29085115256629,-17.3005631050862,55.8360668026083));
#7102=CARTESIAN_POINT('Ctrl Pts',(-6.66439394215464,-17.1834464391567,55.8134832037256));
#7103=CARTESIAN_POINT('Ctrl Pts',(-6.37867965644035,-17.1834464391567,55.8134832037256));
#7104=CARTESIAN_POINT('Ctrl Pts',(-6.37867965644035,-17.1834464391567,55.8134832037256));
#7105=CARTESIAN_POINT('Ctrl Pts',(-6.37867965644035,-17.117907755524,56.153361367358));
#7106=CARTESIAN_POINT('Ctrl Pts',(-6.37867965644035,-17.0393555276599,56.504288680396));
#7107=CARTESIAN_POINT('Ctrl Pts',(-6.37867965644035,-16.9519317131792,56.8453439943512));
#7108=CARTESIAN_POINT('Ctrl Pts',(-8.5,-19.0068161477963,57.3720791843357));
#7109=CARTESIAN_POINT('Ctrl Pts',(-8.5,-19.1048373289154,56.9896817231935));
#7110=CARTESIAN_POINT('Ctrl Pts',(-8.5,-19.1929115247223,56.5962155959693));
#7111=CARTESIAN_POINT('Ctrl Pts',(-8.5,-19.2663946965195,56.2151379773172));
#7112=CARTESIAN_POINT('Ctrl Pts',(-6.37867965644035,-17.1834464391566,55.8134832037259));
#7113=CARTESIAN_POINT('Ctrl Pts',(-6.37867965644035,-17.2671029617921,55.3796474335628));
#7114=CARTESIAN_POINT('Ctrl Pts',(-6.37867965644035,-17.7670670675718,54.4348084088707));
#7115=CARTESIAN_POINT('Ctrl Pts',(-6.37867965644035,-18.7797191983724,54.));
#7116=CARTESIAN_POINT('Ctrl Pts',(-6.37867965644035,-19.3800314873921,54.));
#7117=CARTESIAN_POINT('Ctrl Pts',(-6.66439394215464,-17.1834464391566,55.8134832037259));
#7118=CARTESIAN_POINT('Ctrl Pts',(-6.66439394215464,-17.2670904928921,55.3797120962412));
#7119=CARTESIAN_POINT('Ctrl Pts',(-6.66439394215464,-17.7670945835653,54.4349191596844));
#7120=CARTESIAN_POINT('Ctrl Pts',(-6.66439394215464,-18.7798086741675,54.));
#7121=CARTESIAN_POINT('Ctrl Pts',(-6.66439394215464,-19.3800314873921,54.));
#7122=CARTESIAN_POINT('Ctrl Pts',(-7.29085029793426,-17.3005627451802,55.836066733208));
#7123=CARTESIAN_POINT('Ctrl Pts',(-7.29085029793426,-17.3797815861421,55.4252444112012));
#7124=CARTESIAN_POINT('Ctrl Pts',(-7.29085029793426,-17.8530161833129,54.5306979949696));
#7125=CARTESIAN_POINT('Ctrl Pts',(-7.29085029793426,-18.811563635118,54.1192738233666));
#7126=CARTESIAN_POINT('Ctrl Pts',(-7.29085029793426,-19.3800314873921,54.1192738233666));
#7127=CARTESIAN_POINT('Ctrl Pts',(-8.04465837989033,-17.8781931120305,55.9474511583355));
#7128=CARTESIAN_POINT('Ctrl Pts',(-8.04465837989033,-17.9353929452527,55.6508175795378));
#7129=CARTESIAN_POINT('Ctrl Pts',(-8.04465837989033,-18.277217601953,55.0048072380441));
#7130=CARTESIAN_POINT('Ctrl Pts',(-8.04465837989033,-18.9695702139447,54.7075453005509));
#7131=CARTESIAN_POINT('Ctrl Pts',(-8.04465837989033,-19.3800314873921,54.7075453005509));
#7132=CARTESIAN_POINT('Ctrl Pts',(-8.43400047932411,-18.6073592624962,56.0880562185142));
#7133=CARTESIAN_POINT('Ctrl Pts',(-8.43400047932411,-18.6367767603382,55.9354995208353));
#7134=CARTESIAN_POINT('Ctrl Pts',(-8.43400047932411,-18.8126751779652,55.6031777109637));
#7135=CARTESIAN_POINT('Ctrl Pts',(-8.43400047932411,-19.1689339553594,55.4501441545311));
#7136=CARTESIAN_POINT('Ctrl Pts',(-8.43400047932411,-19.3800314873921,55.4501441545311));
#7137=CARTESIAN_POINT('Ctrl Pts',(-8.5,-19.055985148285,56.1745647181597));
#7138=CARTESIAN_POINT('Ctrl Pts',(-8.5,-19.0683328632447,56.1105304951182));
#7139=CARTESIAN_POINT('Ctrl Pts',(-8.5,-19.1420682054501,55.9711212909647));
#7140=CARTESIAN_POINT('Ctrl Pts',(-8.5,-19.291425305852,55.9070346292739));
#7141=CARTESIAN_POINT('Ctrl Pts',(-8.5,-19.3800314873921,55.9070346292739));
#7142=CARTESIAN_POINT('Ctrl Pts',(-8.5,-19.2663946965196,56.2151379773172));
#7143=CARTESIAN_POINT('Ctrl Pts',(-8.5,-19.2707225320274,56.1926941822423));
#7144=CARTESIAN_POINT('Ctrl Pts',(-8.5,-19.2965873700759,56.143814456532));
#7145=CARTESIAN_POINT('Ctrl Pts',(-8.5,-19.3489752976487,56.1213203435596));
#7146=CARTESIAN_POINT('Ctrl Pts',(-8.5,-19.3800314873921,56.1213203435596));
#7147=CARTESIAN_POINT('',(-8.5,-19.3800314873921,56.1213203435596));
#7148=CARTESIAN_POINT('',(-6.37867965644035,-19.3800314873921,54.));
#7149=CARTESIAN_POINT('Ctrl Pts',(-8.5,-19.3800314873921,56.1213203435596));
#7150=CARTESIAN_POINT('Ctrl Pts',(-8.5,-19.3800314873921,55.9070346292739));
#7151=CARTESIAN_POINT('Ctrl Pts',(-8.43400047932411,-19.3800314873921,55.4501441545311));
#7152=CARTESIAN_POINT('Ctrl Pts',(-8.04465837989033,-19.3800314873921,54.7075453005509));
#7153=CARTESIAN_POINT('Ctrl Pts',(-7.29085029793426,-19.3800314873921,54.1192738233666));
#7154=CARTESIAN_POINT('Ctrl Pts',(-6.66439394215464,-19.3800314873921,54.));
#7155=CARTESIAN_POINT('Ctrl Pts',(-6.37867965644035,-19.3800314873921,54.));
#7156=CARTESIAN_POINT('Ctrl Pts',(-6.37867965644035,-19.3800314873921,54.));
#7157=CARTESIAN_POINT('Ctrl Pts',(-6.37867965644035,-18.7797191983724,54.));
#7158=CARTESIAN_POINT('Ctrl Pts',(-6.37867965644035,-17.7670670675718,54.4348084088707));
#7159=CARTESIAN_POINT('Ctrl Pts',(-6.37867965644035,-17.2671029617921,55.3796474335628));
#7160=CARTESIAN_POINT('Ctrl Pts',(-6.37867965644035,-17.1834464391566,55.8134832037259));
#7161=CARTESIAN_POINT('Ctrl Pts',(-8.5,-19.2663946965196,56.2151379773172));
#7162=CARTESIAN_POINT('Ctrl Pts',(-8.5,-19.2707225320274,56.1926941822423));
#7163=CARTESIAN_POINT('Ctrl Pts',(-8.5,-19.2965873700759,56.143814456532));
#7164=CARTESIAN_POINT('Ctrl Pts',(-8.5,-19.3489752976487,56.1213203435596));
#7165=CARTESIAN_POINT('Ctrl Pts',(-8.5,-19.3800314873921,56.1213203435596));
#7166=CARTESIAN_POINT('Ctrl Pts',(-6.37867965644035,-19.380031542032,54.));
#7167=CARTESIAN_POINT('Ctrl Pts',(-6.37867965644035,-23.5940881839923,54.0000002170871));
#7168=CARTESIAN_POINT('Ctrl Pts',(-6.37867965644035,-27.7891699875342,54.0000004331968));
#7169=CARTESIAN_POINT('Ctrl Pts',(-6.37867965644035,-31.999999845455,54.0000006501177));
#7170=CARTESIAN_POINT('Ctrl Pts',(-6.66439394215464,-19.380031542032,54.));
#7171=CARTESIAN_POINT('Ctrl Pts',(-6.66439394215464,-23.5940881839923,54.0000002170871));
#7172=CARTESIAN_POINT('Ctrl Pts',(-6.66439394215464,-27.7891699875342,54.0000004331968));
#7173=CARTESIAN_POINT('Ctrl Pts',(-6.66439394215464,-31.999999845455,54.0000006501177));
#7174=CARTESIAN_POINT('Ctrl Pts',(-7.29086126549403,-19.3800315358874,54.1192785130262));
#7175=CARTESIAN_POINT('Ctrl Pts',(-7.29086126549403,-23.5940881778477,54.1192787301133));
#7176=CARTESIAN_POINT('Ctrl Pts',(-7.29086126549403,-27.7891699813896,54.1192789462229));
#7177=CARTESIAN_POINT('Ctrl Pts',(-7.29086126549403,-31.9999998393104,54.1192791631438));
#7178=CARTESIAN_POINT('Ctrl Pts',(-8.04466232388412,-19.3800315055827,54.7075464587638));
#7179=CARTESIAN_POINT('Ctrl Pts',(-8.04466232388412,-23.594088147543,54.707546675851));
#7180=CARTESIAN_POINT('Ctrl Pts',(-8.04466232388412,-27.789169951085,54.7075468919606));
#7181=CARTESIAN_POINT('Ctrl Pts',(-8.04466232388412,-31.9999998090057,54.7075471088815));
#7182=CARTESIAN_POINT('Ctrl Pts',(-8.43400552734115,-19.3800314673278,55.4501442725561));
#7183=CARTESIAN_POINT('Ctrl Pts',(-8.43400552734115,-23.5940881092881,55.4501444896432));
#7184=CARTESIAN_POINT('Ctrl Pts',(-8.43400552734115,-27.78916991283,55.4501447057528));
#7185=CARTESIAN_POINT('Ctrl Pts',(-8.43400552734115,-31.9999997707508,55.4501449226738));
#7186=CARTESIAN_POINT('Ctrl Pts',(-8.5,-19.3800314437911,55.9070346292739));
#7187=CARTESIAN_POINT('Ctrl Pts',(-8.5,-23.5940880857514,55.9070348463611));
#7188=CARTESIAN_POINT('Ctrl Pts',(-8.5,-27.7891698892933,55.9070350624707));
#7189=CARTESIAN_POINT('Ctrl Pts',(-8.5,-31.9999997472141,55.9070352793916));
#7190=CARTESIAN_POINT('Ctrl Pts',(-8.5,-19.3800314327522,56.1213203435596));
#7191=CARTESIAN_POINT('Ctrl Pts',(-8.5,-23.5940880747125,56.1213205606468));
#7192=CARTESIAN_POINT('Ctrl Pts',(-8.5,-27.7891698782544,56.1213207767564));
#7193=CARTESIAN_POINT('Ctrl Pts',(-8.5,-31.9999997361752,56.1213209936773));
#7194=CARTESIAN_POINT('',(-8.5,-31.9999997361752,56.1213209936773));
#7195=CARTESIAN_POINT('',(-6.37867965644035,-31.999999845455,54.0000006501177));
#7196=CARTESIAN_POINT('Ctrl Pts',(-8.5,-31.9999997361752,56.1213209936773));
#7197=CARTESIAN_POINT('Ctrl Pts',(-8.5,-31.9999997472141,55.9070352793916));
#7198=CARTESIAN_POINT('Ctrl Pts',(-8.43400552734115,-31.9999997707508,55.4501449226738));
#7199=CARTESIAN_POINT('Ctrl Pts',(-8.04466232388412,-31.9999998090057,54.7075471088815));
#7200=CARTESIAN_POINT('Ctrl Pts',(-7.29086126549403,-31.9999998393104,54.1192791631438));
#7201=CARTESIAN_POINT('Ctrl Pts',(-6.66439394215464,-31.999999845455,54.0000006501177));
#7202=CARTESIAN_POINT('Ctrl Pts',(-6.37867965644035,-31.999999845455,54.0000006501177));
#7203=CARTESIAN_POINT('Ctrl Pts',(-6.37867965644035,-31.999999845455,54.0000006501177));
#7204=CARTESIAN_POINT('Ctrl Pts',(-6.37867965644035,-27.7891699875342,54.0000004331968));
#7205=CARTESIAN_POINT('Ctrl Pts',(-6.37867965644035,-23.5940881839923,54.0000002170871));
#7206=CARTESIAN_POINT('Ctrl Pts',(-6.37867965644035,-19.380031542032,54.));
#7207=CARTESIAN_POINT('Ctrl Pts',(-8.5,-19.3800314873921,56.1213203435597));
#7208=CARTESIAN_POINT('Ctrl Pts',(-8.5,-23.5940881109751,56.1213205606468));
#7209=CARTESIAN_POINT('Ctrl Pts',(-8.5,-27.7891698964537,56.1213207767564));
#7210=CARTESIAN_POINT('Ctrl Pts',(-8.5,-31.9999997361752,56.1213209936773));
#7211=CARTESIAN_POINT('Ctrl Pts',(-6.37867965644035,-31.999999845455,54.0000006501177));
#7212=CARTESIAN_POINT('Ctrl Pts',(-6.37867965644035,-32.6261158828895,54.0000006823721));
#7213=CARTESIAN_POINT('Ctrl Pts',(-6.37867965644035,-33.2502411339106,53.7979493706431));
#7214=CARTESIAN_POINT('Ctrl Pts',(-6.37867965644035,-33.7574178884678,53.4313546690326));
#7215=CARTESIAN_POINT('Ctrl Pts',(-6.66439394215464,-31.999999845455,54.0000006501177));
#7216=CARTESIAN_POINT('Ctrl Pts',(-6.66439394215464,-32.6261854714262,54.0000006823756));
#7217=CARTESIAN_POINT('Ctrl Pts',(-6.66439394215464,-33.2501847646659,53.7979901151494));
#7218=CARTESIAN_POINT('Ctrl Pts',(-6.66439394215464,-33.7574178884678,53.4313546690326));
#7219=CARTESIAN_POINT('Ctrl Pts',(-7.29086279675178,-31.9999998393103,54.1192798154656));
#7220=CARTESIAN_POINT('Ctrl Pts',(-7.29086279675178,-32.6508824379237,54.1192798489958));
#7221=CARTESIAN_POINT('Ctrl Pts',(-7.29086279675178,-33.3000537651981,53.9091203003576));
#7222=CARTESIAN_POINT('Ctrl Pts',(-7.29086279675178,-33.8272923347691,53.5280246283797));
#7223=CARTESIAN_POINT('Ctrl Pts',(-8.04466288268867,-31.9999998090057,54.7075472722757));
#7224=CARTESIAN_POINT('Ctrl Pts',(-8.04466288268867,-32.7737697939603,54.7075473121365));
#7225=CARTESIAN_POINT('Ctrl Pts',(-8.04466288268867,-33.545121098274,54.4578337518026));
#7226=CARTESIAN_POINT('Ctrl Pts',(-8.04466288268867,-34.1719029187029,54.0047867768171));
#7227=CARTESIAN_POINT('Ctrl Pts',(-8.43400623770282,-31.9999997707508,55.4501449429846));
#7228=CARTESIAN_POINT('Ctrl Pts',(-8.43400623770282,-32.9288220914724,55.4501449908329));
#7229=CARTESIAN_POINT('Ctrl Pts',(-8.43400623770282,-33.854541212412,55.1504571029839));
#7230=CARTESIAN_POINT('Ctrl Pts',(-8.43400623770282,-34.6069210621824,54.6066260538554));
#7231=CARTESIAN_POINT('Ctrl Pts',(-8.5,-31.9999997472141,55.9070352793916));
#7232=CARTESIAN_POINT('Ctrl Pts',(-8.5,-33.0240879867551,55.9070353321475));
#7233=CARTESIAN_POINT('Ctrl Pts',(-8.49999999999999,-34.0450214379272,55.5765232560171));
#7234=CARTESIAN_POINT('Ctrl Pts',(-8.49999999999999,-34.8745701456056,54.9769134390642));
#7235=CARTESIAN_POINT('Ctrl Pts',(-8.5,-31.9999997361752,56.1213209936773));
#7236=CARTESIAN_POINT('Ctrl Pts',(-8.5,-33.0688466694893,56.121321048739));
#7237=CARTESIAN_POINT('Ctrl Pts',(-8.5,-34.1342951178172,55.7763978843389));
#7238=CARTESIAN_POINT('Ctrl Pts',(-8.5,-35.0000999947819,55.1505815832724));
#7239=CARTESIAN_POINT('',(-8.5,-35.000099996118,55.1505815851209));
#7240=CARTESIAN_POINT('',(-6.37867965644035,-33.7574178884678,53.4313546690326));
#7241=CARTESIAN_POINT('Ctrl Pts',(-8.5,-35.0000999947819,55.1505815832724));
#7242=CARTESIAN_POINT('Ctrl Pts',(-8.49999999999999,-34.8745701456056,54.9769134390642));
#7243=CARTESIAN_POINT('Ctrl Pts',(-8.43400623770282,-34.6069210621824,54.6066260538554));
#7244=CARTESIAN_POINT('Ctrl Pts',(-8.04466288268867,-34.1719029187029,54.0047867768171));
#7245=CARTESIAN_POINT('Ctrl Pts',(-7.29086279675178,-33.8272923347691,53.5280246283797));
#7246=CARTESIAN_POINT('Ctrl Pts',(-6.66439394215464,-33.7574178884678,53.4313546690326));
#7247=CARTESIAN_POINT('Ctrl Pts',(-6.37867965644035,-33.7574178884678,53.4313546690326));
#7248=CARTESIAN_POINT('Ctrl Pts',(-6.37867965644035,-33.7574178884678,53.4313546690326));
#7249=CARTESIAN_POINT('Ctrl Pts',(-6.37867965644035,-33.2502411339106,53.7979493706431));
#7250=CARTESIAN_POINT('Ctrl Pts',(-6.37867965644035,-32.6261158828895,54.0000006823721));
#7251=CARTESIAN_POINT('Ctrl Pts',(-6.37867965644035,-31.999999845455,54.0000006501177));
#7252=CARTESIAN_POINT('Ctrl Pts',(-8.5,-31.9999997361752,56.1213209936773));
#7253=CARTESIAN_POINT('Ctrl Pts',(-8.5,-33.0688466694893,56.121321048739));
#7254=CARTESIAN_POINT('Ctrl Pts',(-8.5,-34.1342951178172,55.7763978843389));
#7255=CARTESIAN_POINT('Ctrl Pts',(-8.5,-35.0000999947819,55.1505815832724));
#7256=CARTESIAN_POINT('Ctrl Pts',(-6.37867965644035,-33.7574178915313,53.4313546668182));
#7257=CARTESIAN_POINT('Ctrl Pts',(-6.37867965644035,-34.0855855212474,53.1941503518879));
#7258=CARTESIAN_POINT('Ctrl Pts',(-6.37867965644035,-34.7382072200962,52.4834496268985));
#7259=CARTESIAN_POINT('Ctrl Pts',(-6.37867965644035,-35.,51.5400520046389));
#7260=CARTESIAN_POINT('Ctrl Pts',(-6.37867965644035,-35.,51.0000006501177));
#7261=CARTESIAN_POINT('Ctrl Pts',(-6.66439394215464,-33.7574178915313,53.4313546668182));
#7262=CARTESIAN_POINT('Ctrl Pts',(-6.66439394215464,-34.0856219948462,53.1941239882425));
#7263=CARTESIAN_POINT('Ctrl Pts',(-6.66439394215464,-34.7382647569064,52.4834385847507));
#7264=CARTESIAN_POINT('Ctrl Pts',(-6.66439394215464,-35.,51.5401120276717));
#7265=CARTESIAN_POINT('Ctrl Pts',(-6.66439394215464,-35.,51.0000006501177));
#7266=CARTESIAN_POINT('Ctrl Pts',(-7.29086286320516,-33.8272923545303,53.5280246490098));
#7267=CARTESIAN_POINT('Ctrl Pts',(-7.29086286320516,-34.1684409385622,53.2814375123238));
#7268=CARTESIAN_POINT('Ctrl Pts',(-7.29086286320516,-34.846972065121,52.5424514137685));
#7269=CARTESIAN_POINT('Ctrl Pts',(-7.29086286320516,-35.1192791936438,51.5614142028766));
#7270=CARTESIAN_POINT('Ctrl Pts',(-7.29086286320516,-35.1192791936438,51.0000006501177));
#7271=CARTESIAN_POINT('Ctrl Pts',(-8.04466290698454,-34.1719029266483,54.0047867798349));
#7272=CARTESIAN_POINT('Ctrl Pts',(-8.04466290698454,-34.5774607573477,53.711643706952));
#7273=CARTESIAN_POINT('Ctrl Pts',(-8.04466290698454,-35.3839980659312,52.8333217523325));
#7274=CARTESIAN_POINT('Ctrl Pts',(-8.04466290698455,-35.7075466292583,51.6674097300301));
#7275=CARTESIAN_POINT('Ctrl Pts',(-8.04466290698455,-35.7075466292583,51.0000006501177));
#7276=CARTESIAN_POINT('Ctrl Pts',(-8.43400626856183,-34.6069210672554,54.6066260513022));
#7277=CARTESIAN_POINT('Ctrl Pts',(-8.43400626856183,-35.0937468330793,54.2547413380763));
#7278=CARTESIAN_POINT('Ctrl Pts',(-8.43400626856183,-36.0618499111555,53.2005128404082));
#7279=CARTESIAN_POINT('Ctrl Pts',(-8.43400626856183,-36.4501442937695,51.8011488757254));
#7280=CARTESIAN_POINT('Ctrl Pts',(-8.43400626856183,-36.4501442937695,51.0000006501177));
#7281=CARTESIAN_POINT('Ctrl Pts',(-8.5,-34.8745701506165,54.9769134354423));
#7282=CARTESIAN_POINT('Ctrl Pts',(-8.5,-35.4113278602056,54.588937190202));
#7283=CARTESIAN_POINT('Ctrl Pts',(-8.49999999999999,-36.4787960194463,53.4264515481114));
#7284=CARTESIAN_POINT('Ctrl Pts',(-8.5,-36.9070346292739,51.8833197281267));
#7285=CARTESIAN_POINT('Ctrl Pts',(-8.5,-36.9070346292739,51.0000006501177));
#7286=CARTESIAN_POINT('Ctrl Pts',(-8.5,-35.0001000000116,55.1505815794923));
#7287=CARTESIAN_POINT('Ctrl Pts',(-8.5,-35.560317186066,54.745648484948));
#7288=CARTESIAN_POINT('Ctrl Pts',(-8.49999999999999,-36.6744121137202,53.5324064579244));
#7289=CARTESIAN_POINT('Ctrl Pts',(-8.5,-37.1213203435596,51.9219259796098));
#7290=CARTESIAN_POINT('Ctrl Pts',(-8.5,-37.1213203435596,51.0000006501177));
#7291=CARTESIAN_POINT('',(-6.39927708632443,-35.0001000000116,51.0000006501177));
#7292=CARTESIAN_POINT('Ctrl Pts',(-8.5,-35.0001000000116,55.1505815794923));
#7293=CARTESIAN_POINT('Ctrl Pts',(-8.5,-35.0001000000116,54.7942909783228));
#7294=CARTESIAN_POINT('Ctrl Pts',(-8.44252630885498,-35.0001000000116,54.3341755321066));
#7295=CARTESIAN_POINT('Ctrl Pts',(-7.9977864749675,-35.0001000000116,53.1607439828215));
#7296=CARTESIAN_POINT('Ctrl Pts',(-7.64356066430923,-35.0001000000116,52.6053548907106));
#7297=CARTESIAN_POINT('Ctrl Pts',(-7.13512176886221,-35.0001000000116,51.9212185861545));
#7298=CARTESIAN_POINT('Ctrl Pts',(-6.98622001132231,-35.0001000000116,51.733048434934));
#7299=CARTESIAN_POINT('Ctrl Pts',(-6.77438009122045,-35.0001000000116,51.4732179267382));
#7300=CARTESIAN_POINT('Ctrl Pts',(-6.71639805957763,-35.0001000000183,51.4029135245357));
#7301=CARTESIAN_POINT('Ctrl Pts',(-6.56409934304602,-35.0001000000183,51.2192961959561));
#7302=CARTESIAN_POINT('Ctrl Pts',(-6.49554616509506,-35.0001000000116,51.1375362219706));
#7303=CARTESIAN_POINT('Ctrl Pts',(-6.421818278566,-35.0001000000116,51.0464054488998));
#7304=CARTESIAN_POINT('Ctrl Pts',(-6.40818706140854,-35.0001000000116,51.027500080116));
#7305=CARTESIAN_POINT('Ctrl Pts',(-6.40112856488211,-35.0001000000116,51.0110323238185));
#7306=CARTESIAN_POINT('Ctrl Pts',(-6.40013353150608,-35.0001000000116,51.007791289022));
#7307=CARTESIAN_POINT('Ctrl Pts',(-6.39939979873532,-35.0001000000116,51.0030753137652));
#7308=CARTESIAN_POINT('Ctrl Pts',(-6.39927708632375,-35.0001000000116,51.001544338149));
#7309=CARTESIAN_POINT('Ctrl Pts',(-6.39927708632375,-35.0001000000116,51.0000006501177));
#7310=CARTESIAN_POINT('',(-6.37867965644035,-35.,51.0000006501177));
#7311=CARTESIAN_POINT('Ctrl Pts',(-6.39927705543382,-35.0001030896936,51.0000006501177));
#7312=CARTESIAN_POINT('Ctrl Pts',(-6.39239586884655,-35.0000342828437,51.0000006501177));
#7313=CARTESIAN_POINT('Ctrl Pts',(-6.38552985288297,-35.,51.0000006501177));
#7314=CARTESIAN_POINT('Ctrl Pts',(-6.37867965644035,-35.,51.0000006501177));
#7315=CARTESIAN_POINT('Ctrl Pts',(-6.37867965644035,-35.,51.0000006501177));
#7316=CARTESIAN_POINT('Ctrl Pts',(-6.37867965644035,-35.,51.5400520046389));
#7317=CARTESIAN_POINT('Ctrl Pts',(-6.37867965644035,-34.7382072200962,52.4834496268985));
#7318=CARTESIAN_POINT('Ctrl Pts',(-6.37867965644035,-34.0855855212474,53.1941503518879));
#7319=CARTESIAN_POINT('Ctrl Pts',(-6.37867965644035,-33.7574178915313,53.4313546668182));
#7320=CARTESIAN_POINT('Ctrl Pts',(-6.37867965644035,-35.,51.0000006501177));
#7321=CARTESIAN_POINT('Ctrl Pts',(-6.37867965644035,-35.,44.3274205067641));
#7322=CARTESIAN_POINT('Ctrl Pts',(-6.37867965644035,-35.,37.6674518910119));
#7323=CARTESIAN_POINT('Ctrl Pts',(-6.37867965644035,-35.,31.));
#7324=CARTESIAN_POINT('Ctrl Pts',(-6.38553184849945,-35.,51.0000006501177));
#7325=CARTESIAN_POINT('Ctrl Pts',(-6.38553184849945,-35.,44.3274205067641));
#7326=CARTESIAN_POINT('Ctrl Pts',(-6.38553184849945,-35.,37.6674518910119));
#7327=CARTESIAN_POINT('Ctrl Pts',(-6.38553184849945,-35.,31.));
#7328=CARTESIAN_POINT('Ctrl Pts',(-6.39239779355103,-35.0000332008452,51.0000006501177));
#7329=CARTESIAN_POINT('Ctrl Pts',(-6.39239779355103,-35.0000332008452,44.3274205067641));
#7330=CARTESIAN_POINT('Ctrl Pts',(-6.39239779355103,-35.0000332008452,37.6674518910119));
#7331=CARTESIAN_POINT('Ctrl Pts',(-6.39239779355103,-35.0000332008452,31.));
#7332=CARTESIAN_POINT('Ctrl Pts',(-6.39927708632444,-35.0001000000116,51.0000006501177));
#7333=CARTESIAN_POINT('Ctrl Pts',(-6.39927708632444,-35.0001000000116,44.3274205067641));
#7334=CARTESIAN_POINT('Ctrl Pts',(-6.39927708632444,-35.0001000000116,37.6674518910119));
#7335=CARTESIAN_POINT('Ctrl Pts',(-6.39927708632444,-35.0001000000116,31.));
#7336=CARTESIAN_POINT('',(-6.37867965644035,-35.,31.));
#7337=CARTESIAN_POINT('',(-6.39927699932664,-35.0000000027982,31.));
#7338=CARTESIAN_POINT('',(-20.,-35.,31.));
#7339=CARTESIAN_POINT('Ctrl Pts',(-6.37867965644035,-35.,31.));
#7340=CARTESIAN_POINT('Ctrl Pts',(-6.37867965644035,-35.,37.6674518910119));
#7341=CARTESIAN_POINT('Ctrl Pts',(-6.37867965644035,-35.,44.3274205067641));
#7342=CARTESIAN_POINT('Ctrl Pts',(-6.37867965644035,-35.,51.0000006501177));
#7343=CARTESIAN_POINT('Ctrl Pts',(-6.39927708632407,-35.0001000000116,51.0000006501177));
#7344=CARTESIAN_POINT('Ctrl Pts',(-6.39927708632398,-35.0001000000116,46.7650241821894));
#7345=CARTESIAN_POINT('Ctrl Pts',(-6.3992770863239,-35.0001000000116,42.5300477142611));
#7346=CARTESIAN_POINT('Ctrl Pts',(-6.39927708632376,-35.0001000000116,35.8633808308886));
#7347=CARTESIAN_POINT('Ctrl Pts',(-6.39927708632391,-35.0001000000116,33.4316904154443));
#7348=CARTESIAN_POINT('Ctrl Pts',(-6.39927708632403,-35.0001000000116,31.));
#7349=CARTESIAN_POINT('Origin',(-8.5,-5.00000057890304E-5,52.9360395921679));
#7350=CARTESIAN_POINT('',(-8.5,-35.0001000000116,57.3720791843357));
#7351=CARTESIAN_POINT('',(-8.5,17.499924739221,57.3720791843357));
#7352=CARTESIAN_POINT('',(-8.5,-35.0001000000116,74.8720791843357));
#7353=CARTESIAN_POINT('Origin',(-26.,17.499924739221,57.3720791843357));
#7354=CARTESIAN_POINT('',(-8.5,34.9999395751835,57.3720791843357));
#7355=CARTESIAN_POINT('',(-8.5,17.499924739221,57.3720791843357));
#7356=CARTESIAN_POINT('',(-26.,34.9998994784478,74.8720791843345));
#7357=CARTESIAN_POINT('Origin',(-26.,34.9999395751835,57.3720791843357));
#7358=CARTESIAN_POINT('',(-26.,-35.0001000000116,74.8720791843357));
#7359=CARTESIAN_POINT('',(-26.,17.499924739221,74.8720791843357));
#7360=CARTESIAN_POINT('Origin',(-26.,-35.0001000000116,57.3720791843357));
#7361=CARTESIAN_POINT('Origin',(-8.5,-5.00000057890304E-5,52.9360395921679));
#7362=CARTESIAN_POINT('',(-8.5,34.9998994784478,74.8720791843345));
#7363=CARTESIAN_POINT('Ctrl Pts',(-2.12132034355964,35.,51.0000006501177));
#7364=CARTESIAN_POINT('Ctrl Pts',(-2.12132034355964,35.,43.9937759547244));
#7365=CARTESIAN_POINT('Ctrl Pts',(-2.12132034355964,35.,37.0008534541443));
#7366=CARTESIAN_POINT('Ctrl Pts',(-2.12132034355964,35.,30.));
#7367=CARTESIAN_POINT('Ctrl Pts',(-1.83560605784536,35.,51.0000006501177));
#7368=CARTESIAN_POINT('Ctrl Pts',(-1.83560605784536,35.,43.9937759547244));
#7369=CARTESIAN_POINT('Ctrl Pts',(-1.83560605784536,35.,37.0008534541443));
#7370=CARTESIAN_POINT('Ctrl Pts',(-1.83560605784536,35.,30.));
#7371=CARTESIAN_POINT('Ctrl Pts',(-1.20914581904087,34.8807245127738,51.0000006501177));
#7372=CARTESIAN_POINT('Ctrl Pts',(-1.20914581904087,34.8807245127738,43.9937759547244));
#7373=CARTESIAN_POINT('Ctrl Pts',(-1.20914581904087,34.8807245127738,37.0008534541443));
#7374=CARTESIAN_POINT('Ctrl Pts',(-1.20914581904087,34.8807245127738,30.));
#7375=CARTESIAN_POINT('Ctrl Pts',(-0.455340235533083,34.2924542918181,51.0000006501177));
#7376=CARTESIAN_POINT('Ctrl Pts',(-0.455340235533083,34.2924542918181,43.9937759547244));
#7377=CARTESIAN_POINT('Ctrl Pts',(-0.455340235533083,34.2924542918181,37.0008534541443));
#7378=CARTESIAN_POINT('Ctrl Pts',(-0.455340235533083,34.2924542918181,30.));
#7379=CARTESIAN_POINT('Ctrl Pts',(-0.065997741473231,33.5498558092142,51.0000006501177));
#7380=CARTESIAN_POINT('Ctrl Pts',(-0.065997741473231,33.5498558092142,43.9937759547244));
#7381=CARTESIAN_POINT('Ctrl Pts',(-0.065997741473231,33.5498558092142,37.0008534541443));
#7382=CARTESIAN_POINT('Ctrl Pts',(-0.065997741473231,33.5498558092142,30.));
#7383=CARTESIAN_POINT('Ctrl Pts',(0.,33.0929653707261,51.0000006501177));
#7384=CARTESIAN_POINT('Ctrl Pts',(0.,33.0929653707261,43.9937759547244));
#7385=CARTESIAN_POINT('Ctrl Pts',(0.,33.0929653707261,37.0008534541443));
#7386=CARTESIAN_POINT('Ctrl Pts',(0.,33.0929653707261,30.));
#7387=CARTESIAN_POINT('Ctrl Pts',(0.,32.8786796564404,51.0000006501177));
#7388=CARTESIAN_POINT('Ctrl Pts',(0.,32.8786796564404,43.9937759547244));
#7389=CARTESIAN_POINT('Ctrl Pts',(0.,32.8786796564404,37.0008534541443));
#7390=CARTESIAN_POINT('Ctrl Pts',(0.,32.8786796564404,30.));
#7391=CARTESIAN_POINT('',(0.,32.8786796564404,30.));
#7392=CARTESIAN_POINT('',(-2.12132034355964,35.,30.));
#7393=CARTESIAN_POINT('Ctrl Pts',(0.,32.8786796564404,30.));
#7394=CARTESIAN_POINT('Ctrl Pts',(0.,33.0929653707261,30.));
#7395=CARTESIAN_POINT('Ctrl Pts',(-0.0329988707366155,33.3214105899701,
30.));
#7396=CARTESIAN_POINT('Ctrl Pts',(-0.107899680213901,33.5470229719827,30.));
#7397=CARTESIAN_POINT('Ctrl Pts',(-0.182800489691187,33.7726353539953,30.));
#7398=CARTESIAN_POINT('Ctrl Pts',(-0.299603237909142,33.9954148987765,30.));
#7399=CARTESIAN_POINT('Ctrl Pts',(-0.454454811586546,34.1914763527892,30.));
#7400=CARTESIAN_POINT('Ctrl Pts',(-0.660923576489751,34.452891624806,30.));
#7401=CARTESIAN_POINT('Ctrl Pts',(-0.935034697765309,34.6668080687899,30.));
#7402=CARTESIAN_POINT('Ctrl Pts',(-1.22870531810421,34.8035851625884,30.));
#7403=CARTESIAN_POINT('Ctrl Pts',(-1.52237593844311,34.9403622563869,30.));
#7404=CARTESIAN_POINT('Ctrl Pts',(-1.83560605784536,35.,30.));
#7405=CARTESIAN_POINT('Ctrl Pts',(-2.12132034355964,35.,30.));
#7406=CARTESIAN_POINT('',(-2.12132034355964,35.,51.0000006501177));
#7407=CARTESIAN_POINT('Ctrl Pts',(-2.12132034355964,35.,30.));
#7408=CARTESIAN_POINT('Ctrl Pts',(-2.12132034355964,35.,37.0008534541443));
#7409=CARTESIAN_POINT('Ctrl Pts',(-2.12132034355964,35.,43.9937759547244));
#7410=CARTESIAN_POINT('Ctrl Pts',(-2.12132034355964,35.,51.0000006501177));
#7411=CARTESIAN_POINT('',(0.,32.8786796564404,51.0000006501177));
#7412=CARTESIAN_POINT('Ctrl Pts',(-2.12132034355964,35.,51.0000006501177));
#7413=CARTESIAN_POINT('Ctrl Pts',(-1.83560605784536,35.,51.0000006501177));
#7414=CARTESIAN_POINT('Ctrl Pts',(-1.20914581904087,34.8807245127738,51.0000006501177));
#7415=CARTESIAN_POINT('Ctrl Pts',(-0.455340235533083,34.2924542918181,51.0000006501177));
#7416=CARTESIAN_POINT('Ctrl Pts',(-0.065997741473231,33.5498558092142,51.0000006501177));
#7417=CARTESIAN_POINT('Ctrl Pts',(0.,33.0929653707261,51.0000006501177));
#7418=CARTESIAN_POINT('Ctrl Pts',(0.,32.8786796564404,51.0000006501177));
#7419=CARTESIAN_POINT('Ctrl Pts',(0.,32.8786796564404,51.0000006501177));
#7420=CARTESIAN_POINT('Ctrl Pts',(0.,32.8786796564404,43.9937759547244));
#7421=CARTESIAN_POINT('Ctrl Pts',(0.,32.8786796564404,37.0008534541443));
#7422=CARTESIAN_POINT('Ctrl Pts',(0.,32.8786796564404,30.));
#7423=CARTESIAN_POINT('Ctrl Pts',(0.,32.8786796564404,51.0000006501177));
#7424=CARTESIAN_POINT('Ctrl Pts',(0.,32.8786796564404,51.197241629744));
#7425=CARTESIAN_POINT('Ctrl Pts',(0.,32.7177646664625,51.6577375903093));
#7426=CARTESIAN_POINT('Ctrl Pts',(0.,32.2629836704437,51.8786803201109));
#7427=CARTESIAN_POINT('Ctrl Pts',(0.,31.9999999547173,51.8786803065581));
#7428=CARTESIAN_POINT('Ctrl Pts',(-3.73831537781851E-17,33.1643939421546,
51.0000006501177));
#7429=CARTESIAN_POINT('Ctrl Pts',(-3.73831537781851E-17,33.1643939421547,
51.2609089327107));
#7430=CARTESIAN_POINT('Ctrl Pts',(-9.25965981612066E-17,32.9508157063449,
51.8707913380558));
#7431=CARTESIAN_POINT('Ctrl Pts',(3.73831537781852E-17,32.3478720188586,
52.1643946101999));
#7432=CARTESIAN_POINT('Ctrl Pts',(3.73831537781851E-17,31.9999999399931,
52.1643945922723));
#7433=CARTESIAN_POINT('Ctrl Pts',(-0.119275961933236,33.7908552904515,51.0000006501177));
#7434=CARTESIAN_POINT('Ctrl Pts',(-0.119275961933236,33.7908552904515,51.4020865730021));
#7435=CARTESIAN_POINT('Ctrl Pts',(-0.119275961933236,33.4629527404772,52.3406964768753));
#7436=CARTESIAN_POINT('Ctrl Pts',(-0.119275961933235,32.5361057932183,52.7908559681974));
#7437=CARTESIAN_POINT('Ctrl Pts',(-0.119275961933235,31.9999999077085,52.7908559405692));
#7438=CARTESIAN_POINT('Ctrl Pts',(-0.707545825143674,34.5446601624604,51.0000006501177));
#7439=CARTESIAN_POINT('Ctrl Pts',(-0.707545825143674,34.5446601624604,51.5711387670255));
#7440=CARTESIAN_POINT('Ctrl Pts',(-0.707545825143674,34.0785969586992,52.9046828234336));
#7441=CARTESIAN_POINT('Ctrl Pts',(-0.707545825143674,32.7615050310335,53.5446608518222));
#7442=CARTESIAN_POINT('Ctrl Pts',(-0.707545825143674,31.9999998688612,53.5446608125781));
#7443=CARTESIAN_POINT('Ctrl Pts',(-1.45014420226184,34.9340027685158,51.0000006501176));
#7444=CARTESIAN_POINT('Ctrl Pts',(-1.45014420226184,34.9340027685159,51.658581172531));
#7445=CARTESIAN_POINT('Ctrl Pts',(-1.45014420226184,34.3966708419147,53.1962044391584));
#7446=CARTESIAN_POINT('Ctrl Pts',(-1.45014420226184,32.8780929976815,53.934003463886));
#7447=CARTESIAN_POINT('Ctrl Pts',(-1.45014420226184,31.9999998487964,53.9340034186335));
#7448=CARTESIAN_POINT('Ctrl Pts',(-1.90703462927393,35.,51.0000006501176));
#7449=CARTESIAN_POINT('Ctrl Pts',(-1.90703462927393,35.,51.6734462278452));
#7450=CARTESIAN_POINT('Ctrl Pts',(-1.90703462927393,34.4506183606249,53.2456947831434));
#7451=CARTESIAN_POINT('Ctrl Pts',(-1.90703462927393,32.8979127471959,54.0000006963915));
#7452=CARTESIAN_POINT('Ctrl Pts',(-1.90703462927393,31.9999998453953,54.0000006501177));
#7453=CARTESIAN_POINT('Ctrl Pts',(-2.12132034355964,35.,51.0000006501176));
#7454=CARTESIAN_POINT('Ctrl Pts',(-2.12132034355964,35.,51.6734234778136));
#7455=CARTESIAN_POINT('Ctrl Pts',(-2.12132034355964,34.4506018588285,53.2456550317936));
#7456=CARTESIAN_POINT('Ctrl Pts',(-2.12132034355964,32.8978824143115,54.00000069639));
#7457=CARTESIAN_POINT('Ctrl Pts',(-2.12132034355964,31.9999998453953,54.0000006501177));
#7458=CARTESIAN_POINT('',(-2.12132034355964,31.9999998453953,54.0000006501177));
#7459=CARTESIAN_POINT('',(0.,31.9999999547173,51.8786803065581));
#7460=CARTESIAN_POINT('Ctrl Pts',(-2.12132034355964,31.9999998453953,54.0000006501177));
#7461=CARTESIAN_POINT('Ctrl Pts',(-1.90703462927393,31.9999998453953,54.0000006501177));
#7462=CARTESIAN_POINT('Ctrl Pts',(-1.45014420226184,31.9999998487964,53.9340034186335));
#7463=CARTESIAN_POINT('Ctrl Pts',(-0.707545825143674,31.9999998688612,53.5446608125781));
#7464=CARTESIAN_POINT('Ctrl Pts',(-0.119275961933235,31.9999999077085,52.7908559405692));
#7465=CARTESIAN_POINT('Ctrl Pts',(3.73831537781851E-17,31.9999999399931,
52.1643945922723));
#7466=CARTESIAN_POINT('Ctrl Pts',(0.,31.9999999547173,51.8786803065581));
#7467=CARTESIAN_POINT('Ctrl Pts',(0.,31.9999999547173,51.8786803065581));
#7468=CARTESIAN_POINT('Ctrl Pts',(0.,32.2629836704437,51.8786803201109));
#7469=CARTESIAN_POINT('Ctrl Pts',(0.,32.7177646664625,51.6577375903093));
#7470=CARTESIAN_POINT('Ctrl Pts',(0.,32.8786796564404,51.197241629744));
#7471=CARTESIAN_POINT('Ctrl Pts',(0.,32.8786796564404,51.0000006501177));
#7472=CARTESIAN_POINT('Ctrl Pts',(-2.12132034355964,35.,51.0000006501176));
#7473=CARTESIAN_POINT('Ctrl Pts',(-2.12132034355964,35.,51.6734234778136));
#7474=CARTESIAN_POINT('Ctrl Pts',(-2.12132034355964,34.4506018588285,53.2456550317936));
#7475=CARTESIAN_POINT('Ctrl Pts',(-2.12132034355964,32.8978824143115,54.00000069639));
#7476=CARTESIAN_POINT('Ctrl Pts',(-2.12132034355964,31.9999998453953,54.0000006501177));
#7477=CARTESIAN_POINT('Ctrl Pts',(-2.12132034355964,19.3800314873921,54.));
#7478=CARTESIAN_POINT('Ctrl Pts',(-2.12132034355964,23.5890030900407,54.0000002168252));
#7479=CARTESIAN_POINT('Ctrl Pts',(-2.12132034355964,27.7896866308398,54.0000004332234));
#7480=CARTESIAN_POINT('Ctrl Pts',(-2.12132034355964,31.9999998454164,54.0000006501177));
#7481=CARTESIAN_POINT('Ctrl Pts',(-1.83560605784536,19.3800314873921,54.));
#7482=CARTESIAN_POINT('Ctrl Pts',(-1.83560605784536,23.5890030900407,54.0000002168252));
#7483=CARTESIAN_POINT('Ctrl Pts',(-1.83560605784536,27.7896866308398,54.0000004332234));
#7484=CARTESIAN_POINT('Ctrl Pts',(-1.83560605784536,31.9999998454164,54.0000006501177));
#7485=CARTESIAN_POINT('Ctrl Pts',(-1.20914581904101,19.3800314935366,53.8807245127739));
#7486=CARTESIAN_POINT('Ctrl Pts',(-1.20914581904101,23.5890030961852,53.880724729599));
#7487=CARTESIAN_POINT('Ctrl Pts',(-1.20914581904101,27.7896866369843,53.8807249459973));
#7488=CARTESIAN_POINT('Ctrl Pts',(-1.20914581904101,31.9999998515609,53.8807251628916));
#7489=CARTESIAN_POINT('Ctrl Pts',(-0.455340235533132,19.3800315238413,53.2924542918181));
#7490=CARTESIAN_POINT('Ctrl Pts',(-0.455340235533132,23.5890031264899,53.2924545086433));
#7491=CARTESIAN_POINT('Ctrl Pts',(-0.455340235533132,27.789686667289,53.2924547250415));
#7492=CARTESIAN_POINT('Ctrl Pts',(-0.455340235533132,31.9999998818656,53.2924549419358));
#7493=CARTESIAN_POINT('Ctrl Pts',(-0.0659977414732951,19.3800315620963,
52.5498558092142));
#7494=CARTESIAN_POINT('Ctrl Pts',(-0.0659977414732951,23.5890031647449,
52.5498560260394));
#7495=CARTESIAN_POINT('Ctrl Pts',(-0.0659977414732951,27.789686705544,52.5498562424376));
#7496=CARTESIAN_POINT('Ctrl Pts',(-0.0659977414732951,31.9999999201206,
52.5498564593319));
#7497=CARTESIAN_POINT('Ctrl Pts',(0.,19.380031585633,52.0929653707261));
#7498=CARTESIAN_POINT('Ctrl Pts',(0.,23.5890031882816,52.0929655875513));
#7499=CARTESIAN_POINT('Ctrl Pts',(0.,27.7896867290807,52.0929658039495));
#7500=CARTESIAN_POINT('Ctrl Pts',(0.,31.9999999436573,52.0929660208438));
#7501=CARTESIAN_POINT('Ctrl Pts',(0.,19.3800315966719,51.8786796564404));
#7502=CARTESIAN_POINT('Ctrl Pts',(0.,23.5890031993205,51.8786798732655));
#7503=CARTESIAN_POINT('Ctrl Pts',(0.,27.7896867401197,51.8786800896638));
#7504=CARTESIAN_POINT('Ctrl Pts',(0.,31.9999999546962,51.8786803065581));
#7505=CARTESIAN_POINT('',(-2.12132034355964,19.3800314873921,54.));
#7506=CARTESIAN_POINT('',(0.,19.3800315966719,51.8786796564404));
#7507=CARTESIAN_POINT('Ctrl Pts',(-2.12132034355964,19.3800314873921,54.));
#7508=CARTESIAN_POINT('Ctrl Pts',(-1.83560605784536,19.3800314873921,54.));
#7509=CARTESIAN_POINT('Ctrl Pts',(-1.20914581904101,19.3800314935366,53.8807245127739));
#7510=CARTESIAN_POINT('Ctrl Pts',(-0.455340235533132,19.3800315238413,53.2924542918181));
#7511=CARTESIAN_POINT('Ctrl Pts',(-0.0659977414732951,19.3800315620963,
52.5498558092142));
#7512=CARTESIAN_POINT('Ctrl Pts',(0.,19.380031585633,52.0929653707261));
#7513=CARTESIAN_POINT('Ctrl Pts',(0.,19.3800315966719,51.8786796564404));
#7514=CARTESIAN_POINT('Ctrl Pts',(0.,19.3800315966719,51.8786796564404));
#7515=CARTESIAN_POINT('Ctrl Pts',(0.,23.5890031993205,51.8786798732655));
#7516=CARTESIAN_POINT('Ctrl Pts',(0.,27.7896867401197,51.8786800896638));
#7517=CARTESIAN_POINT('Ctrl Pts',(0.,31.9999999546962,51.8786803065581));
#7518=CARTESIAN_POINT('Ctrl Pts',(-2.12132034355964,31.9999998454164,54.0000006501177));
#7519=CARTESIAN_POINT('Ctrl Pts',(-2.12132034355964,27.7896866308398,54.0000004332234));
#7520=CARTESIAN_POINT('Ctrl Pts',(-2.12132034355964,23.5890030900407,54.0000002168252));
#7521=CARTESIAN_POINT('Ctrl Pts',(-2.12132034355964,19.3800314873921,54.));
#7522=CARTESIAN_POINT('Ctrl Pts',(-2.12132034355964,17.1834464391567,55.8134832037256));
#7523=CARTESIAN_POINT('Ctrl Pts',(-2.12132034355964,17.2948185578093,55.2359166572309));
#7524=CARTESIAN_POINT('Ctrl Pts',(-2.12132034355964,17.9085541458132,54.3129857845921));
#7525=CARTESIAN_POINT('Ctrl Pts',(-2.12132034355964,18.9389109206226,53.9999999944698));
#7526=CARTESIAN_POINT('Ctrl Pts',(-2.12132034355964,19.3800315154375,54.));
#7527=CARTESIAN_POINT('Ctrl Pts',(-1.83560605784536,17.1834464391567,55.8134832037256));
#7528=CARTESIAN_POINT('Ctrl Pts',(-1.83560605784536,17.2948351576842,55.2358305716603));
#7529=CARTESIAN_POINT('Ctrl Pts',(-1.83560605784536,17.9084593986477,54.3129449535617));
#7530=CARTESIAN_POINT('Ctrl Pts',(-1.83560605784536,18.9388451721502,53.999999994469));
#7531=CARTESIAN_POINT('Ctrl Pts',(-1.83560605784536,19.3800315154375,54.));
#7532=CARTESIAN_POINT('Ctrl Pts',(-1.20915886354306,17.0663340027465,55.7909004204208));
#7533=CARTESIAN_POINT('Ctrl Pts',(-1.20915886354306,17.1836140170936,55.182696018109));
#7534=CARTESIAN_POINT('Ctrl Pts',(-1.20915886354306,17.830272469493,54.2104767085283));
#7535=CARTESIAN_POINT('Ctrl Pts',(-1.20915886354306,18.9155110398637,53.8807301117093));
#7536=CARTESIAN_POINT('Ctrl Pts',(-1.20915886354306,19.3800315169327,53.8807301175329));
#7537=CARTESIAN_POINT('Ctrl Pts',(-0.455344835080339,16.4887007002353,55.6795154292099));
#7538=CARTESIAN_POINT('Ctrl Pts',(-0.455344835080338,16.6352946696137,54.9192912936266));
#7539=CARTESIAN_POINT('Ctrl Pts',(-0.455344835080339,17.4431682391696,53.7044423926936));
#7540=CARTESIAN_POINT('Ctrl Pts',(-0.455344835080339,18.7994048849769,53.2924556433277));
#7541=CARTESIAN_POINT('Ctrl Pts',(-0.455344835080339,19.3800315243078,53.2924556506069));
#7542=CARTESIAN_POINT('Ctrl Pts',(-0.0660036833952015,15.7595336759884,
55.5389102005399));
#7543=CARTESIAN_POINT('Ctrl Pts',(-0.0660036833952008,15.9431143315799,
54.5868761857799));
#7544=CARTESIAN_POINT('Ctrl Pts',(-0.0660036833952016,16.9546119118218,
53.0657000116183));
#7545=CARTESIAN_POINT('Ctrl Pts',(-0.0660036833952013,18.6529087225342,
52.5498558976328));
#7546=CARTESIAN_POINT('Ctrl Pts',(-0.0660036833952013,19.3800315336176,
52.5498559067486));
#7547=CARTESIAN_POINT('Ctrl Pts',(-5.60747306672777E-17,15.3109077300283,
55.4524016892915));
#7548=CARTESIAN_POINT('Ctrl Pts',(1.86449826034637E-16,15.5172134263537,
54.3825175029234));
#7549=CARTESIAN_POINT('Ctrl Pts',(-9.24282552765687E-17,16.6542024147445,
52.6727855991653));
#7550=CARTESIAN_POINT('Ctrl Pts',(3.84627697622366E-25,18.5628998139399,
52.0929653604819));
#7551=CARTESIAN_POINT('Ctrl Pts',(0.,19.3800315393455,52.0929653707261));
#7552=CARTESIAN_POINT('Ctrl Pts',(0.,15.1004981817938,55.411828430134));
#7553=CARTESIAN_POINT('Ctrl Pts',(0.,15.3174807618546,54.2865748125202));
#7554=CARTESIAN_POINT('Ctrl Pts',(0.,16.513201315358,52.4884594099794));
#7555=CARTESIAN_POINT('Ctrl Pts',(0.,18.5206110161515,51.878679645666));
#7556=CARTESIAN_POINT('Ctrl Pts',(0.,19.380031542032,51.8786796564404));
#7557=CARTESIAN_POINT('',(-2.12132034355964,17.1834464391567,55.8134832037256));
#7558=CARTESIAN_POINT('',(0.,15.1004981817938,55.411828430134));
#7559=CARTESIAN_POINT('Ctrl Pts',(-2.12132034355964,17.1834464391567,55.8134832037256));
#7560=CARTESIAN_POINT('Ctrl Pts',(-1.83560605784536,17.1834464391567,55.8134832037256));
#7561=CARTESIAN_POINT('Ctrl Pts',(-1.20915886354306,17.0663340027465,55.7909004204208));
#7562=CARTESIAN_POINT('Ctrl Pts',(-0.455344835080339,16.4887007002353,55.6795154292099));
#7563=CARTESIAN_POINT('Ctrl Pts',(-0.0660036833952015,15.7595336759884,
55.5389102005399));
#7564=CARTESIAN_POINT('Ctrl Pts',(-5.60747306672777E-17,15.3109077300283,
55.4524016892915));
#7565=CARTESIAN_POINT('Ctrl Pts',(0.,15.1004981817938,55.411828430134));
#7566=CARTESIAN_POINT('Ctrl Pts',(0.,15.1004981817938,55.411828430134));
#7567=CARTESIAN_POINT('Ctrl Pts',(0.,15.3174807618546,54.2865748125202));
#7568=CARTESIAN_POINT('Ctrl Pts',(0.,16.513201315358,52.4884594099794));
#7569=CARTESIAN_POINT('Ctrl Pts',(0.,18.5206110161515,51.878679645666));
#7570=CARTESIAN_POINT('Ctrl Pts',(0.,19.380031542032,51.8786796564404));
#7571=CARTESIAN_POINT('Ctrl Pts',(-2.12132034355964,19.3800314873921,54.));
#7572=CARTESIAN_POINT('Ctrl Pts',(-2.12132034355964,18.9389109019061,54.0000000001552));
#7573=CARTESIAN_POINT('Ctrl Pts',(-2.12132034355964,17.9085541402389,54.3129857929746));
#7574=CARTESIAN_POINT('Ctrl Pts',(-2.12132034355964,17.2948185578093,55.2359166572309));
#7575=CARTESIAN_POINT('Ctrl Pts',(-2.12132034355964,17.1834464391567,55.8134832037256));
#7576=CARTESIAN_POINT('Ctrl Pts',(0.,15.1004981817938,55.411828430134));
#7577=CARTESIAN_POINT('Ctrl Pts',(0.,14.7181964939568,57.3944131940254));
#7578=CARTESIAN_POINT('Ctrl Pts',(0.,13.1646620788738,61.2084161039849));
#7579=CARTESIAN_POINT('Ctrl Pts',(0.,8.80253592739979,65.5998831653219));
#7580=CARTESIAN_POINT('Ctrl Pts',(0.,3.09380188060513,67.9778956726815));
#7581=CARTESIAN_POINT('Ctrl Pts',(0.,-3.09300712501298,67.9763940235175));
#7582=CARTESIAN_POINT('Ctrl Pts',(0.,-8.8047766566707,65.6006044096256));
#7583=CARTESIAN_POINT('Ctrl Pts',(0.,-13.1629136545454,61.2080147890074));
#7584=CARTESIAN_POINT('Ctrl Pts',(0.,-14.7181965532993,57.3944130163886));
#7585=CARTESIAN_POINT('Ctrl Pts',(0.,-15.1004982173208,55.4118282458939));
#7586=CARTESIAN_POINT('Ctrl Pts',(0.,15.3810442461065,55.4659261090107));
#7587=CARTESIAN_POINT('Ctrl Pts',(0.,14.9916917803054,57.4850756211365));
#7588=CARTESIAN_POINT('Ctrl Pts',(7.09861723931544E-17,13.4088733048439,
61.3703002831808));
#7589=CARTESIAN_POINT('Ctrl Pts',(-4.54970976055E-17,8.96607423593895,65.8431115317411));
#7590=CARTESIAN_POINT('Ctrl Pts',(1.74366918355959E-17,3.15118170663562,
68.2651806906037));
#7591=CARTESIAN_POINT('Ctrl Pts',(-1.82945629040309E-17,-3.1504293962536,
68.2638373394039));
#7592=CARTESIAN_POINT('Ctrl Pts',(3.3983836790065E-17,-8.96823047064176,
65.8437131532327));
#7593=CARTESIAN_POINT('Ctrl Pts',(-7.83977616403127E-17,-13.4072864799347,
61.3698938985013));
#7594=CARTESIAN_POINT('Ctrl Pts',(0.,-14.9916918407472,57.4850754401985));
#7595=CARTESIAN_POINT('Ctrl Pts',(0.,-15.3810442822936,55.4659259213477));
#7596=CARTESIAN_POINT('Ctrl Pts',(-0.119271769306436,15.9961640790422,55.584539625384));
#7597=CARTESIAN_POINT('Ctrl Pts',(-0.119271769306436,15.5911770229754,57.6847688225764));
#7598=CARTESIAN_POINT('Ctrl Pts',(-0.119271769306436,13.9455752772508,61.7249266531959));
#7599=CARTESIAN_POINT('Ctrl Pts',(-0.119271769306436,9.3246466833128,66.3769129854858));
#7600=CARTESIAN_POINT('Ctrl Pts',(-0.119271769306436,3.27732498131823,68.8959971218407));
#7601=CARTESIAN_POINT('Ctrl Pts',(-0.119271769306436,-3.27647243413541,
68.8943717375029));
#7602=CARTESIAN_POINT('Ctrl Pts',(-0.119271769306436,-9.32704380078624,
66.3777017761324));
#7603=CARTESIAN_POINT('Ctrl Pts',(-0.119271769306436,-13.9436870123243,
61.7245010904894));
#7604=CARTESIAN_POINT('Ctrl Pts',(-0.119271769306436,-15.5911770858384,
57.6847686344034));
#7605=CARTESIAN_POINT('Ctrl Pts',(-0.119271769306436,-15.9961641166764,
55.584539430216));
#7606=CARTESIAN_POINT('Ctrl Pts',(-0.707544802288016,16.7363397346456,55.7272676477045));
#7607=CARTESIAN_POINT('Ctrl Pts',(-0.707544802288016,16.3126311460358,57.9245851559279));
#7608=CARTESIAN_POINT('Ctrl Pts',(-0.707544802288016,14.5907371808805,62.1518158552224));
#7609=CARTESIAN_POINT('Ctrl Pts',(-0.707544802288017,9.75611724712778,67.0189745688111));
#7610=CARTESIAN_POINT('Ctrl Pts',(-0.707544802288016,3.42893923539705,69.6545789430513));
#7611=CARTESIAN_POINT('Ctrl Pts',(-0.707544802288016,-3.42806716335815,
69.6529431938856));
#7612=CARTESIAN_POINT('Ctrl Pts',(-0.707544802288016,-9.75858135999868,
67.0197535318122));
#7613=CARTESIAN_POINT('Ctrl Pts',(-0.707544802288017,-14.5888291335536,
62.1513714318578));
#7614=CARTESIAN_POINT('Ctrl Pts',(-0.707544802288016,-16.3126312118065,
57.9245849590475));
#7615=CARTESIAN_POINT('Ctrl Pts',(-0.707544802288016,-16.7363397740212,
55.7272674435056));
#7616=CARTESIAN_POINT('Ctrl Pts',(-1.45014411828137,17.1186386297034,55.8009863181496));
#7617=CARTESIAN_POINT('Ctrl Pts',(-1.45014411828137,16.685246310872,58.0485228460791));
#7618=CARTESIAN_POINT('Ctrl Pts',(-1.45014411828137,14.9240622829779,62.3722774913806));
#7619=CARTESIAN_POINT('Ctrl Pts',(-1.45014411828137,9.97897084989204,67.3506383401551));
#7620=CARTESIAN_POINT('Ctrl Pts',(-1.45014411828137,3.50727446402829,70.0464587202164));
#7621=CARTESIAN_POINT('Ctrl Pts',(-1.45014411828137,-3.50637674445434,70.044766966671));
#7622=CARTESIAN_POINT('Ctrl Pts',(-1.45014411828137,-9.98150387523715,67.3514484132735));
#7623=CARTESIAN_POINT('Ctrl Pts',(-1.45014411828137,-14.9220912218402,62.3718226774245));
#7624=CARTESIAN_POINT('Ctrl Pts',(-1.45014411828137,-16.6852463781453,58.0485226447015));
#7625=CARTESIAN_POINT('Ctrl Pts',(-1.45014411828137,-17.1186386699785,55.8009861092864));
#7626=CARTESIAN_POINT('Ctrl Pts',(-1.90703462927393,17.1834464391567,55.8134832037256));
#7627=CARTESIAN_POINT('Ctrl Pts',(-1.90703462927393,16.7484079032003,58.0695568767787));
#7628=CARTESIAN_POINT('Ctrl Pts',(-1.90703462927393,14.9806009228527,62.4096420606667));
#7629=CARTESIAN_POINT('Ctrl Pts',(-1.90703462927393,10.0167493251233,67.4068756953095));
#7630=CARTESIAN_POINT('Ctrl Pts',(-1.90703462927393,3.520562743488,70.1129149705606));
#7631=CARTESIAN_POINT('Ctrl Pts',(-1.90703462927393,-3.51965558020761,70.1111971380699));
#7632=CARTESIAN_POINT('Ctrl Pts',(-1.90703462927393,-10.0193052668116,67.4077028909198));
#7633=CARTESIAN_POINT('Ctrl Pts',(-1.90703462927393,-14.9786018920781,62.4091852727419));
#7634=CARTESIAN_POINT('Ctrl Pts',(-1.90703462927393,-16.7484079707286,58.0695566746388));
#7635=CARTESIAN_POINT('Ctrl Pts',(-1.90703462927393,-17.1834464795842,55.8134829940716));
#7636=CARTESIAN_POINT('Ctrl Pts',(-2.12132034355964,17.1834464391567,55.8134832037256));
#7637=CARTESIAN_POINT('Ctrl Pts',(-2.12132034355964,16.748410422632,58.0695438112154));
#7638=CARTESIAN_POINT('Ctrl Pts',(-2.12132034355964,14.9805829581613,62.4096466298823));
#7639=CARTESIAN_POINT('Ctrl Pts',(-2.12132034355964,10.0167493029862,67.4068684519269));
#7640=CARTESIAN_POINT('Ctrl Pts',(-2.12132034355964,3.52055794906399,70.1129017271154));
#7641=CARTESIAN_POINT('Ctrl Pts',(-2.12132034355964,-3.5196535656466,70.1111929419039));
#7642=CARTESIAN_POINT('Ctrl Pts',(-2.12132034355964,-10.0192991163067,67.4076891839791));
#7643=CARTESIAN_POINT('Ctrl Pts',(-2.12132034355964,-14.9785933578555,62.4091899579011));
#7644=CARTESIAN_POINT('Ctrl Pts',(-2.12132034355964,-16.7484104901601,58.0695436090755));
#7645=CARTESIAN_POINT('Ctrl Pts',(-2.12132034355964,-17.1834464795842,55.8134829940716));
#7646=CARTESIAN_POINT('',(-2.12132034355964,-17.1834464391567,55.8134832037256));
#7647=CARTESIAN_POINT('',(0.,-15.1004981817938,55.411828430134));
#7648=CARTESIAN_POINT('Ctrl Pts',(-2.12132034355964,-17.1834464795842,55.8134829940716));
#7649=CARTESIAN_POINT('Ctrl Pts',(-1.90703462927393,-17.1834464795842,55.8134829940716));
#7650=CARTESIAN_POINT('Ctrl Pts',(-1.45014411828137,-17.1186386699785,55.8009861092864));
#7651=CARTESIAN_POINT('Ctrl Pts',(-0.707544802288016,-16.7363397740212,
55.7272674435056));
#7652=CARTESIAN_POINT('Ctrl Pts',(-0.119271769306436,-15.9961641166764,
55.584539430216));
#7653=CARTESIAN_POINT('Ctrl Pts',(0.,-15.3810442822936,55.4659259213477));
#7654=CARTESIAN_POINT('Ctrl Pts',(0.,-15.1004982173208,55.4118282458939));
#7655=CARTESIAN_POINT('Ctrl Pts',(0.,-15.1004981462668,55.411828614374));
#7656=CARTESIAN_POINT('Ctrl Pts',(0.,-14.7181964569451,57.3944132526519));
#7657=CARTESIAN_POINT('Ctrl Pts',(0.,-13.1629135645458,61.2080148797186));
#7658=CARTESIAN_POINT('Ctrl Pts',(0.,-8.8047766566707,65.6006044096256));
#7659=CARTESIAN_POINT('Ctrl Pts',(0.,-3.09300712501298,67.9763940235175));
#7660=CARTESIAN_POINT('Ctrl Pts',(0.,3.09380188060513,67.9778956726815));
#7661=CARTESIAN_POINT('Ctrl Pts',(0.,8.80253592739979,65.5998831653219));
#7662=CARTESIAN_POINT('Ctrl Pts',(0.,13.1646620788738,61.2084161039849));
#7663=CARTESIAN_POINT('Ctrl Pts',(0.,14.7181964939568,57.3944131940254));
#7664=CARTESIAN_POINT('Ctrl Pts',(0.,15.1004981817938,55.411828430134));
#7665=CARTESIAN_POINT('Ctrl Pts',(-2.12132034355964,17.1834464391567,55.8134832037256));
#7666=CARTESIAN_POINT('Ctrl Pts',(-2.12132034355964,16.748410422632,58.0695438112154));
#7667=CARTESIAN_POINT('Ctrl Pts',(-2.12132034355964,14.9805829581613,62.4096466298823));
#7668=CARTESIAN_POINT('Ctrl Pts',(-2.12132034355964,10.0167493029862,67.4068684519269));
#7669=CARTESIAN_POINT('Ctrl Pts',(-2.12132034355964,3.52055794906399,70.1129017271154));
#7670=CARTESIAN_POINT('Ctrl Pts',(-2.12132034355964,-3.5196535656466,70.1111929419039));
#7671=CARTESIAN_POINT('Ctrl Pts',(-2.12132034355964,-10.0192991163067,67.4076891839791));
#7672=CARTESIAN_POINT('Ctrl Pts',(-2.12132034355964,-14.9785932554414,62.4091900611248));
#7673=CARTESIAN_POINT('Ctrl Pts',(-2.12132034355964,-16.748410380515,58.0695438779288));
#7674=CARTESIAN_POINT('Ctrl Pts',(-2.12132034355964,-17.1834463987291,55.8134834133795));
#7675=CARTESIAN_POINT('Ctrl Pts',(-2.12132034355964,-19.3800314873921,54.));
#7676=CARTESIAN_POINT('Ctrl Pts',(-2.12132034355964,-18.9389108965653,54.));
#7677=CARTESIAN_POINT('Ctrl Pts',(-2.12132034355964,-17.9085541350523,54.3129857971382));
#7678=CARTESIAN_POINT('Ctrl Pts',(-2.12132034355964,-17.2948185567905,55.2359166625147));
#7679=CARTESIAN_POINT('Ctrl Pts',(-2.12132034355964,-17.1834464391567,55.8134832037256));
#7680=CARTESIAN_POINT('Ctrl Pts',(-1.83560605784536,-19.3800314873921,54.));
#7681=CARTESIAN_POINT('Ctrl Pts',(-1.83560605784536,-18.9388451480935,54.));
#7682=CARTESIAN_POINT('Ctrl Pts',(-1.83560605784536,-17.9084593878876,54.3129449661094));
#7683=CARTESIAN_POINT('Ctrl Pts',(-1.83560605784536,-17.2948351566652,55.2358305769448));
#7684=CARTESIAN_POINT('Ctrl Pts',(-1.83560605784536,-17.1834464391567,55.8134832037256));
#7685=CARTESIAN_POINT('Ctrl Pts',(-1.20915886354309,-19.3800314873921,53.8807301175329));
#7686=CARTESIAN_POINT('Ctrl Pts',(-1.20915886354309,-18.9155110145227,53.8807301175329));
#7687=CARTESIAN_POINT('Ctrl Pts',(-1.20915886354309,-17.8302724581569,54.2104767217406));
#7688=CARTESIAN_POINT('Ctrl Pts',(-1.20915886354309,-17.1836140160207,55.1826960236731));
#7689=CARTESIAN_POINT('Ctrl Pts',(-1.20915886354309,-17.0663340027465,55.7909004204208));
#7690=CARTESIAN_POINT('Ctrl Pts',(-0.45534483508035,-19.3800314873921,53.2924556506069));
#7691=CARTESIAN_POINT('Ctrl Pts',(-0.45534483508035,-18.7994048533105,53.2924556506069));
#7692=CARTESIAN_POINT('Ctrl Pts',(-0.455344835080351,-17.443168225005,53.7044424092076));
#7693=CARTESIAN_POINT('Ctrl Pts',(-0.45534483508035,-16.6352946682726,54.9192913005814));
#7694=CARTESIAN_POINT('Ctrl Pts',(-0.45534483508035,-16.4887007002353,55.6795154292099));
#7695=CARTESIAN_POINT('Ctrl Pts',(-0.0660036833952163,-19.3800314873921,
52.5498559067486));
#7696=CARTESIAN_POINT('Ctrl Pts',(-0.0660036833952163,-18.6529086828825,
52.5498559067486));
#7697=CARTESIAN_POINT('Ctrl Pts',(-0.0660036833952168,-16.9546118940859,
53.0657000322986));
#7698=CARTESIAN_POINT('Ctrl Pts',(-0.0660036833952163,-15.9431143299004,
54.5868761944894));
#7699=CARTESIAN_POINT('Ctrl Pts',(-0.0660036833952163,-15.7595336759884,
55.5389102005399));
#7700=CARTESIAN_POINT('Ctrl Pts',(0.,-19.3800314873921,52.0929653707261));
#7701=CARTESIAN_POINT('Ctrl Pts',(1.70917049581581E-32,-18.562899769374,
52.0929653707261));
#7702=CARTESIAN_POINT('Ctrl Pts',(-1.87111548691343E-16,-16.6542023948098,
52.672785622406));
#7703=CARTESIAN_POINT('Ctrl Pts',(-2.42907311579532E-18,-15.5172134244663,
54.382517512711));
#7704=CARTESIAN_POINT('Ctrl Pts',(0.,-15.3109077300283,55.4524016892915));
#7705=CARTESIAN_POINT('Ctrl Pts',(0.,-19.3800314873921,51.8786796564404));
#7706=CARTESIAN_POINT('Ctrl Pts',(0.,-18.5206109692815,51.8786796564404));
#7707=CARTESIAN_POINT('Ctrl Pts',(0.,-16.5132012943929,52.4884594344227));
#7708=CARTESIAN_POINT('Ctrl Pts',(0.,-15.3174807598696,54.2865748228144));
#7709=CARTESIAN_POINT('Ctrl Pts',(0.,-15.1004981817938,55.411828430134));
#7710=CARTESIAN_POINT('',(-2.12132034355964,-19.3800314873921,54.));
#7711=CARTESIAN_POINT('',(0.,-19.3800314873921,51.8786796564404));
#7712=CARTESIAN_POINT('Ctrl Pts',(-2.12132034355964,-19.3800314873921,54.));
#7713=CARTESIAN_POINT('Ctrl Pts',(-1.83560605784536,-19.3800314873921,54.));
#7714=CARTESIAN_POINT('Ctrl Pts',(-1.20915886354309,-19.3800314873921,53.8807301175329));
#7715=CARTESIAN_POINT('Ctrl Pts',(-0.45534483508035,-19.3800314873921,53.2924556506069));
#7716=CARTESIAN_POINT('Ctrl Pts',(-0.0660036833952163,-19.3800314873921,
52.5498559067486));
#7717=CARTESIAN_POINT('Ctrl Pts',(0.,-19.3800314873921,52.0929653707261));
#7718=CARTESIAN_POINT('Ctrl Pts',(0.,-19.3800314873921,51.8786796564404));
#7719=CARTESIAN_POINT('Ctrl Pts',(0.,-19.3800314873921,51.8786796564404));
#7720=CARTESIAN_POINT('Ctrl Pts',(0.,-18.5206109692815,51.8786796564404));
#7721=CARTESIAN_POINT('Ctrl Pts',(0.,-16.5132012943929,52.4884594344227));
#7722=CARTESIAN_POINT('Ctrl Pts',(0.,-15.3174807598696,54.2865748228144));
#7723=CARTESIAN_POINT('Ctrl Pts',(0.,-15.1004981817938,55.411828430134));
#7724=CARTESIAN_POINT('Ctrl Pts',(-2.12132034355964,-17.1834464391567,55.8134832037256));
#7725=CARTESIAN_POINT('Ctrl Pts',(-2.12132034355964,-17.2948185567905,55.2359166625147));
#7726=CARTESIAN_POINT('Ctrl Pts',(-2.12132034355964,-17.9085541350523,54.3129857971382));
#7727=CARTESIAN_POINT('Ctrl Pts',(-2.12132034355964,-18.9389108965653,54.));
#7728=CARTESIAN_POINT('Ctrl Pts',(-2.12132034355964,-19.3800314873921,54.));
#7729=CARTESIAN_POINT('Ctrl Pts',(0.,-19.380031542032,51.8786796564404));
#7730=CARTESIAN_POINT('Ctrl Pts',(0.,-23.5890031639361,51.8786798732655));
#7731=CARTESIAN_POINT('Ctrl Pts',(0.,-27.7896867219788,51.8786800896638));
#7732=CARTESIAN_POINT('Ctrl Pts',(0.,-31.9999999547658,51.8786803065581));
#7733=CARTESIAN_POINT('Ctrl Pts',(0.,-19.3800315273134,52.1643939421546));
#7734=CARTESIAN_POINT('Ctrl Pts',(0.,-23.5890031492176,52.1643941589798));
#7735=CARTESIAN_POINT('Ctrl Pts',(0.,-27.7896867072603,52.164394375378));
#7736=CARTESIAN_POINT('Ctrl Pts',(0.,-31.9999999400472,52.1643945922723));
#7737=CARTESIAN_POINT('Ctrl Pts',(-0.119275487226149,-19.3800314950413,
52.790854180959));
#7738=CARTESIAN_POINT('Ctrl Pts',(-0.119275487226149,-23.5890031169454,
52.7908543977842));
#7739=CARTESIAN_POINT('Ctrl Pts',(-0.119275487226149,-27.7896866749881,
52.7908546141824));
#7740=CARTESIAN_POINT('Ctrl Pts',(-0.119275487226149,-31.9999999077751,
52.7908548310767));
#7741=CARTESIAN_POINT('Ctrl Pts',(-0.707545708181871,-19.380031456209,53.5446597644669));
#7742=CARTESIAN_POINT('Ctrl Pts',(-0.707545708181871,-23.5890030781132,
53.544659981292));
#7743=CARTESIAN_POINT('Ctrl Pts',(-0.707545708181871,-27.7896866361559,
53.5446601976903));
#7744=CARTESIAN_POINT('Ctrl Pts',(-0.707545708181871,-31.9999998689428,
53.5446604145846));
#7745=CARTESIAN_POINT('Ctrl Pts',(-1.45014419078584,-19.380031436152,53.9340022585267));
#7746=CARTESIAN_POINT('Ctrl Pts',(-1.45014419078584,-23.5890030580562,53.9340024753519));
#7747=CARTESIAN_POINT('Ctrl Pts',(-1.45014419078584,-27.7896866160989,53.9340026917501));
#7748=CARTESIAN_POINT('Ctrl Pts',(-1.45014419078584,-31.9999998488858,53.9340029086444));
#7749=CARTESIAN_POINT('Ctrl Pts',(-1.90703462927393,-19.3800314327522,54.));
#7750=CARTESIAN_POINT('Ctrl Pts',(-1.90703462927393,-23.5890030546563,54.0000002168252));
#7751=CARTESIAN_POINT('Ctrl Pts',(-1.90703462927393,-27.789686612699,54.0000004332234));
#7752=CARTESIAN_POINT('Ctrl Pts',(-1.90703462927393,-31.999999845486,54.0000006501177));
#7753=CARTESIAN_POINT('Ctrl Pts',(-2.12132034355964,-19.3800314327522,54.));
#7754=CARTESIAN_POINT('Ctrl Pts',(-2.12132034355964,-23.5890030546563,54.0000002168252));
#7755=CARTESIAN_POINT('Ctrl Pts',(-2.12132034355964,-27.789686612699,54.0000004332234));
#7756=CARTESIAN_POINT('Ctrl Pts',(-2.12132034355964,-31.999999845486,54.0000006501177));
#7757=CARTESIAN_POINT('',(-2.12132034355964,-31.999999845486,54.0000006501177));
#7758=CARTESIAN_POINT('',(0.,-31.9999999547658,51.8786803065581));
#7759=CARTESIAN_POINT('Ctrl Pts',(-2.12132034355964,-31.999999845486,54.0000006501177));
#7760=CARTESIAN_POINT('Ctrl Pts',(-1.90703462927393,-31.999999845486,54.0000006501177));
#7761=CARTESIAN_POINT('Ctrl Pts',(-1.45014419078584,-31.9999998488858,53.9340029086444));
#7762=CARTESIAN_POINT('Ctrl Pts',(-0.707545708181871,-31.9999998689428,
53.5446604145846));
#7763=CARTESIAN_POINT('Ctrl Pts',(-0.119275487226149,-31.9999999077751,
52.7908548310767));
#7764=CARTESIAN_POINT('Ctrl Pts',(0.,-31.9999999400472,52.1643945922723));
#7765=CARTESIAN_POINT('Ctrl Pts',(0.,-31.9999999547658,51.8786803065581));
#7766=CARTESIAN_POINT('Ctrl Pts',(0.,-31.9999999547658,51.8786803065581));
#7767=CARTESIAN_POINT('Ctrl Pts',(0.,-27.7896867219788,51.8786800896638));
#7768=CARTESIAN_POINT('Ctrl Pts',(0.,-23.5890031639361,51.8786798732655));
#7769=CARTESIAN_POINT('Ctrl Pts',(0.,-19.380031542032,51.8786796564404));
#7770=CARTESIAN_POINT('Ctrl Pts',(-2.12132034355964,-19.3800314873921,54.));
#7771=CARTESIAN_POINT('Ctrl Pts',(-2.12132034355964,-23.5890030910112,54.0000002168252));
#7772=CARTESIAN_POINT('Ctrl Pts',(-2.12132034355964,-27.7896866309181,54.0000004332234));
#7773=CARTESIAN_POINT('Ctrl Pts',(-2.12132034355964,-31.999999845486,54.0000006501177));
#7774=CARTESIAN_POINT('Ctrl Pts',(0.,-31.9999999547548,51.8786803065581));
#7775=CARTESIAN_POINT('Ctrl Pts',(0.,-32.1972377415442,51.8786803167143));
#7776=CARTESIAN_POINT('Ctrl Pts',(0.,-32.6577149440455,51.7177834826772));
#7777=CARTESIAN_POINT('Ctrl Pts',(0.,-32.8786796564446,51.2629886229218));
#7778=CARTESIAN_POINT('Ctrl Pts',(0.,-32.8786796564404,51.0000006501034));
#7779=CARTESIAN_POINT('Ctrl Pts',(0.,-31.9999999400427,52.1643945922723));
#7780=CARTESIAN_POINT('Ctrl Pts',(0.,-32.2609039991848,52.1643946057069));
#7781=CARTESIAN_POINT('Ctrl Pts',(-9.08192836805913E-17,-32.8707615917812,
51.9508403862498));
#7782=CARTESIAN_POINT('Ctrl Pts',(3.52858375230007E-16,-33.1643939421603,
51.3478783602006));
#7783=CARTESIAN_POINT('Ctrl Pts',(0.,-33.1643939421546,51.0000006500987));
#7784=CARTESIAN_POINT('Ctrl Pts',(-0.119275961933235,-31.9999999077849,
52.7908559405692));
#7785=CARTESIAN_POINT('Ctrl Pts',(-0.119275961933235,-32.4020793219062,
52.7908559612732));
#7786=CARTESIAN_POINT('Ctrl Pts',(-0.119275961933236,-33.3406509864574,
52.4629904231461));
#7787=CARTESIAN_POINT('Ctrl Pts',(-0.119275961933234,-33.7908552904603,
51.5361152139003));
#7788=CARTESIAN_POINT('Ctrl Pts',(-0.119275961933235,-33.7908552904515,
51.0000006500885));
#7789=CARTESIAN_POINT('Ctrl Pts',(-0.707545825143674,-31.9999998689697,
53.5446608125781));
#7790=CARTESIAN_POINT('Ctrl Pts',(-0.707545825143674,-32.5711287405834,
53.5446608419868));
#7791=CARTESIAN_POINT('Ctrl Pts',(-0.707545825143674,-33.9046184804968,
53.078650211204));
#7792=CARTESIAN_POINT('Ctrl Pts',(-0.707545825143673,-34.5446601624728,
51.7615181392383));
#7793=CARTESIAN_POINT('Ctrl Pts',(-0.707545825143674,-34.5446601624604,
51.0000006500762));
#7794=CARTESIAN_POINT('Ctrl Pts',(-1.45014420226184,-31.9999998489216,53.9340034186335));
#7795=CARTESIAN_POINT('Ctrl Pts',(-1.45014420226184,-32.6585697105674,53.9340034525448));
#7796=CARTESIAN_POINT('Ctrl Pts',(-1.45014420226184,-34.1961303447082,53.3967321479677));
#7797=CARTESIAN_POINT('Ctrl Pts',(-1.45014420226184,-34.9340027685302,51.8781080132318));
#7798=CARTESIAN_POINT('Ctrl Pts',(-1.45014420226184,-34.9340027685158,51.0000006500698));
#7799=CARTESIAN_POINT('Ctrl Pts',(-1.90703462927393,-31.9999998455233,54.0000006501177));
#7800=CARTESIAN_POINT('Ctrl Pts',(-1.90703462927393,-32.6734345218553,54.0000006847944));
#7801=CARTESIAN_POINT('Ctrl Pts',(-1.90703462927393,-34.2456190309428,53.4506810357792));
#7802=CARTESIAN_POINT('Ctrl Pts',(-1.90703462927393,-35.0000000000147,51.8979280869818));
#7803=CARTESIAN_POINT('Ctrl Pts',(-1.90703462927393,-35.,51.0000006500687));
#7804=CARTESIAN_POINT('Ctrl Pts',(-2.12132034355964,-31.9999998455233,54.0000006501177));
#7805=CARTESIAN_POINT('Ctrl Pts',(-2.12132034355964,-32.673411772192,54.0000006847932));
#7806=CARTESIAN_POINT('Ctrl Pts',(-2.12132034355964,-34.2455792821355,53.4506645318811));
#7807=CARTESIAN_POINT('Ctrl Pts',(-2.12132034355964,-35.0000000000147,51.8978977536063));
#7808=CARTESIAN_POINT('Ctrl Pts',(-2.12132034355964,-35.,51.0000006500687));
#7809=CARTESIAN_POINT('',(-2.12132034355964,-35.,51.0000006500688));
#7810=CARTESIAN_POINT('',(0.,-32.8786796564404,51.0000006501034));
#7811=CARTESIAN_POINT('Ctrl Pts',(-2.12132034355964,-35.,51.0000006500687));
#7812=CARTESIAN_POINT('Ctrl Pts',(-1.90703462927393,-35.,51.0000006500687));
#7813=CARTESIAN_POINT('Ctrl Pts',(-1.45014420226184,-34.9340027685158,51.0000006500698));
#7814=CARTESIAN_POINT('Ctrl Pts',(-0.707545825143674,-34.5446601624604,
51.0000006500762));
#7815=CARTESIAN_POINT('Ctrl Pts',(-0.119275961933235,-33.7908552904515,
51.0000006500885));
#7816=CARTESIAN_POINT('Ctrl Pts',(0.,-33.1643939421546,51.0000006500987));
#7817=CARTESIAN_POINT('Ctrl Pts',(0.,-32.8786796564404,51.0000006501034));
#7818=CARTESIAN_POINT('Ctrl Pts',(0.,-32.8786796564404,51.0000006501034));
#7819=CARTESIAN_POINT('Ctrl Pts',(0.,-32.8786796564446,51.2629886229218));
#7820=CARTESIAN_POINT('Ctrl Pts',(0.,-32.6577149440455,51.7177834826772));
#7821=CARTESIAN_POINT('Ctrl Pts',(0.,-32.1972377415442,51.8786803167143));
#7822=CARTESIAN_POINT('Ctrl Pts',(0.,-31.9999999547548,51.8786803065581));
#7823=CARTESIAN_POINT('Ctrl Pts',(-2.12132034355964,-31.9999998455233,54.0000006501177));
#7824=CARTESIAN_POINT('Ctrl Pts',(-2.12132034355964,-32.673411772192,54.0000006847932));
#7825=CARTESIAN_POINT('Ctrl Pts',(-2.12132034355964,-34.2455792821355,53.4506645318811));
#7826=CARTESIAN_POINT('Ctrl Pts',(-2.12132034355964,-35.0000000000147,51.8978977536063));
#7827=CARTESIAN_POINT('Ctrl Pts',(-2.12132034355964,-35.,51.0000006500687));
#7828=CARTESIAN_POINT('Ctrl Pts',(0.,-32.8786796564404,51.0000006500861));
#7829=CARTESIAN_POINT('Ctrl Pts',(0.,-32.8786796564404,43.9937759550453));
#7830=CARTESIAN_POINT('Ctrl Pts',(0.,-32.8786796564404,37.0008502462934));
#7831=CARTESIAN_POINT('Ctrl Pts',(0.,-32.8786796564404,30.));
#7832=CARTESIAN_POINT('Ctrl Pts',(0.,-33.1643939421546,51.0000006500861));
#7833=CARTESIAN_POINT('Ctrl Pts',(0.,-33.1643939421546,43.9937759550453));
#7834=CARTESIAN_POINT('Ctrl Pts',(0.,-33.1643939421546,37.0008502462934));
#7835=CARTESIAN_POINT('Ctrl Pts',(0.,-33.1643939421546,30.));
#7836=CARTESIAN_POINT('Ctrl Pts',(-0.119275487226208,-33.7908541809591,
51.0000006500861));
#7837=CARTESIAN_POINT('Ctrl Pts',(-0.119275487226208,-33.7908541809591,
43.9937759550453));
#7838=CARTESIAN_POINT('Ctrl Pts',(-0.119275487226208,-33.7908541809591,
37.0008502462934));
#7839=CARTESIAN_POINT('Ctrl Pts',(-0.119275487226208,-33.7908541809591,
30.));
#7840=CARTESIAN_POINT('Ctrl Pts',(-0.707545708181886,-34.5446597644669,
51.0000006500861));
#7841=CARTESIAN_POINT('Ctrl Pts',(-0.707545708181886,-34.5446597644669,
43.9937759550453));
#7842=CARTESIAN_POINT('Ctrl Pts',(-0.707545708181886,-34.5446597644669,
37.0008502462934));
#7843=CARTESIAN_POINT('Ctrl Pts',(-0.707545708181886,-34.5446597644669,
30.));
#7844=CARTESIAN_POINT('Ctrl Pts',(-1.45014419078585,-34.9340022585268,51.0000006500861));
#7845=CARTESIAN_POINT('Ctrl Pts',(-1.45014419078585,-34.9340022585268,43.9937759550453));
#7846=CARTESIAN_POINT('Ctrl Pts',(-1.45014419078585,-34.9340022585268,37.0008502462934));
#7847=CARTESIAN_POINT('Ctrl Pts',(-1.45014419078585,-34.9340022585268,30.));
#7848=CARTESIAN_POINT('Ctrl Pts',(-1.90703462927393,-35.,51.0000006500861));
#7849=CARTESIAN_POINT('Ctrl Pts',(-1.90703462927393,-35.,43.9937759550453));
#7850=CARTESIAN_POINT('Ctrl Pts',(-1.90703462927393,-35.,37.0008502462934));
#7851=CARTESIAN_POINT('Ctrl Pts',(-1.90703462927393,-35.,30.));
#7852=CARTESIAN_POINT('Ctrl Pts',(-2.12132034355964,-35.,51.0000006500861));
#7853=CARTESIAN_POINT('Ctrl Pts',(-2.12132034355964,-35.,43.9937759550453));
#7854=CARTESIAN_POINT('Ctrl Pts',(-2.12132034355964,-35.,37.0008502462934));
#7855=CARTESIAN_POINT('Ctrl Pts',(-2.12132034355964,-35.,30.));
#7856=CARTESIAN_POINT('',(-2.12132034355964,-35.,30.));
#7857=CARTESIAN_POINT('',(0.,-32.8786796564404,30.));
#7858=CARTESIAN_POINT('Ctrl Pts',(-2.12132034355964,-35.,30.));
#7859=CARTESIAN_POINT('Ctrl Pts',(-1.90703462927393,-35.,30.));
#7860=CARTESIAN_POINT('Ctrl Pts',(-1.67858941002989,-34.9670011292634,30.));
#7861=CARTESIAN_POINT('Ctrl Pts',(-1.45297702801727,-34.8921003197861,30.));
#7862=CARTESIAN_POINT('Ctrl Pts',(-1.22736464600466,-34.8171995103088,30.));
#7863=CARTESIAN_POINT('Ctrl Pts',(-1.00458510122347,-34.7003967620909,30.));
#7864=CARTESIAN_POINT('Ctrl Pts',(-0.808523647210829,-34.5455451884135,
30.));
#7865=CARTESIAN_POINT('Ctrl Pts',(-0.547108375193974,-34.3390764235102,
30.));
#7866=CARTESIAN_POINT('Ctrl Pts',(-0.333191931210091,-34.0649653022347,
30.));
#7867=CARTESIAN_POINT('Ctrl Pts',(-0.196414837411598,-33.7712946818958,
30.));
#7868=CARTESIAN_POINT('Ctrl Pts',(-0.0596377436131043,-33.4776240615569,
30.));
#7869=CARTESIAN_POINT('Ctrl Pts',(0.,-33.1643939421546,30.));
#7870=CARTESIAN_POINT('Ctrl Pts',(0.,-32.8786796564404,30.));
#7871=CARTESIAN_POINT('Ctrl Pts',(0.,-32.8786796564404,30.));
#7872=CARTESIAN_POINT('Ctrl Pts',(0.,-32.8786796564404,37.0008502462934));
#7873=CARTESIAN_POINT('Ctrl Pts',(0.,-32.8786796564404,43.9937759550453));
#7874=CARTESIAN_POINT('Ctrl Pts',(0.,-32.8786796564404,51.0000006500861));
#7875=CARTESIAN_POINT('Ctrl Pts',(-2.12132034355964,-35.,51.0000006500861));
#7876=CARTESIAN_POINT('Ctrl Pts',(-2.12132034355964,-35.,43.9937759550453));
#7877=CARTESIAN_POINT('Ctrl Pts',(-2.12132034355964,-35.,37.0008502462934));
#7878=CARTESIAN_POINT('Ctrl Pts',(-2.12132034355964,-35.,30.));
#7879=CARTESIAN_POINT('Origin',(0.,-35.,30.));
#7880=CARTESIAN_POINT('',(-40.,-35.,31.));
#7881=CARTESIAN_POINT('',(-20.,-35.,31.));
#7882=CARTESIAN_POINT('',(-40.1715728752538,-35.,30.));
#7883=CARTESIAN_POINT('Origin',(-43.,-35.,31.));
#7884=CARTESIAN_POINT('',(0.,-35.,30.));
#7885=CARTESIAN_POINT('',(0.,-35.,51.0000006501177));
#7886=CARTESIAN_POINT('Origin',(0.,-32.,51.0000006501177));
#7887=CARTESIAN_POINT('',(0.,-31.999999845455,54.0000006501177));
#7888=CARTESIAN_POINT('Origin',(0.,-31.999999845455,54.0000006501177));
#7889=CARTESIAN_POINT('',(0.,-19.3800314873921,54.));
#7890=CARTESIAN_POINT('Origin',(0.,-19.3800314873921,56.2370505521246));
#7891=CARTESIAN_POINT('',(0.,-17.1834460733662,55.8134831331902));
#7892=CARTESIAN_POINT('Origin',(0.,0.,52.500000372529));
#7893=CARTESIAN_POINT('',(0.,17.1834464391567,55.8134832037256));
#7894=CARTESIAN_POINT('Origin',(0.,19.3800314873921,56.2370505521246));
#7895=CARTESIAN_POINT('',(0.,19.3800314873921,54.));
#7896=CARTESIAN_POINT('Origin',(0.,19.3800314873921,54.));
#7897=CARTESIAN_POINT('',(0.,31.999999845455,54.0000006501177));
#7898=CARTESIAN_POINT('Origin',(0.,32.,51.0000006501177));
#7899=CARTESIAN_POINT('',(-40.,35.,51.0000006501177));
#7900=CARTESIAN_POINT('',(0.,35.,51.0000006501177));
#7901=CARTESIAN_POINT('',(-40.,34.9999541371497,51.0165890494702));
#7902=CARTESIAN_POINT('Origin',(-40.,32.,51.0000006501177));
#7903=CARTESIAN_POINT('',(0.,34.9999541371497,51.0165890496373));
#7904=CARTESIAN_POINT('Origin',(0.,35.,51.0000006501177));
#7905=CARTESIAN_POINT('',(-40.1715728752538,35.,30.));
#7906=CARTESIAN_POINT('',(0.,35.,30.));
#7907=CARTESIAN_POINT('',(-40.,35.,31.));
#7908=CARTESIAN_POINT('Origin',(-43.,35.,31.));
#7909=CARTESIAN_POINT('',(-40.,35.,41.0000003250588));
#7910=CARTESIAN_POINT('Origin',(0.,35.,30.));
#7911=CARTESIAN_POINT('',(0.,12.5,30.));
#7912=CARTESIAN_POINT('',(0.,12.5,30.));
#7913=CARTESIAN_POINT('',(-40.1715728752538,12.5,30.));
#7914=CARTESIAN_POINT('',(0.,12.5,30.));
#7915=CARTESIAN_POINT('',(-40.1715728752538,-12.5,30.));
#7916=CARTESIAN_POINT('Origin',(-40.,-35.0001000000116,74.8720791843357));
#7917=CARTESIAN_POINT('',(-40.,-35.0001000000116,74.8720791843357));
#7918=CARTESIAN_POINT('',(-40.,-35.0001000000116,74.8720791843357));
#7919=CARTESIAN_POINT('',(-40.,-35.0001000000116,74.8720791843357));
#7920=CARTESIAN_POINT('Origin',(-40.,34.9998994784478,74.8720791843357));
#7921=CARTESIAN_POINT('',(-40.,34.9998994784478,74.8720791843345));
#7922=CARTESIAN_POINT('',(-40.,34.9998994784478,74.8720791843345));
#7923=CARTESIAN_POINT('',(-40.,-35.0001000000116,74.8720791843357));
#7924=CARTESIAN_POINT('Origin',(-40.,34.9999541371497,51.0165890494702));
#7925=CARTESIAN_POINT('',(-40.,34.9998994784478,74.8720791843345));
#7926=CARTESIAN_POINT('Origin',(-40.,-12.5,31.));
#7927=CARTESIAN_POINT('',(-40.,-12.5,31.));
#7928=CARTESIAN_POINT('Origin',(-43.,-12.5,31.));
#7929=CARTESIAN_POINT('',(-43.,12.5,28.));
#7930=CARTESIAN_POINT('Origin',(-43.,12.5,31.));
#7931=CARTESIAN_POINT('',(-43.,-12.5,28.));
#7932=CARTESIAN_POINT('',(-43.,-12.5,28.));
#7933=CARTESIAN_POINT('',(-40.1715728752538,-12.5,30.));
#7934=CARTESIAN_POINT('Origin',(-43.,-12.5,31.));
#7935=CARTESIAN_POINT('',(-40.1715728752538,-12.5,30.));
#7936=CARTESIAN_POINT('Origin',(-54.1954416479917,-12.5,28.));
#7937=CARTESIAN_POINT('',(-54.1954416479917,12.5,28.));
#7938=CARTESIAN_POINT('',(-27.0977208239958,12.5,28.));
#7939=CARTESIAN_POINT('',(-54.1954416479917,-12.5,28.));
#7940=CARTESIAN_POINT('',(-54.1954416479917,-12.5,28.));
#7941=CARTESIAN_POINT('',(-27.0977208239958,-12.5,28.));
#7942=CARTESIAN_POINT('Origin',(-54.1954416479917,-12.5,25.));
#7943=CARTESIAN_POINT('',(-57.0932191268589,12.5,25.7764571353076));
#7944=CARTESIAN_POINT('Origin',(-54.1954416479917,12.5,25.));
#7945=CARTESIAN_POINT('',(-57.0932191268589,-12.5,25.7764571353076));
#7946=CARTESIAN_POINT('',(-57.0932191268589,-12.5,25.7764571353076));
#7947=CARTESIAN_POINT('Origin',(-54.1954416479917,-12.5,25.));
#7948=CARTESIAN_POINT('Origin',(-59.9807621135332,-12.5,15.));
#7949=CARTESIAN_POINT('',(-57.3012701892219,12.5,25.));
#7950=CARTESIAN_POINT('',(-56.0967875173176,12.5,29.4951905283833));
#7951=CARTESIAN_POINT('',(-57.3012701892219,7.,25.));
#7952=CARTESIAN_POINT('',(-57.3012701892219,0.,25.));
#7953=CARTESIAN_POINT('',(-59.9807621135332,7.,15.));
#7954=CARTESIAN_POINT('',(-56.7217875173176,7.,27.1626587736527));
#7955=CARTESIAN_POINT('',(-59.9807621135332,-7.,15.));
#7956=CARTESIAN_POINT('',(-59.9807621135332,-12.5,15.));
#7957=CARTESIAN_POINT('',(-57.3012701892219,-7.,25.));
#7958=CARTESIAN_POINT('',(-57.9717875173176,-7.,22.4975952641916));
#7959=CARTESIAN_POINT('',(-57.3012701892219,-12.5,25.));
#7960=CARTESIAN_POINT('',(-57.3012701892219,-9.75,25.));
#7961=CARTESIAN_POINT('',(-56.7217875173176,-12.5,27.1626587736527));
#7962=CARTESIAN_POINT('Origin',(0.,-12.5,30.));
#7963=CARTESIAN_POINT('',(0.,-12.5,30.));
#7964=CARTESIAN_POINT('',(0.,-12.5,30.));
#7965=CARTESIAN_POINT('',(0.,-12.5,30.));
#7966=CARTESIAN_POINT('Origin',(0.,-12.5,25.));
#7967=CARTESIAN_POINT('',(0.,-12.5,25.));
#7968=CARTESIAN_POINT('',(0.,-12.5,25.));
#7969=CARTESIAN_POINT('',(0.,-12.5,25.));
#7970=CARTESIAN_POINT('Origin',(0.,-7.,25.));
#7971=CARTESIAN_POINT('',(0.,-7.,25.));
#7972=CARTESIAN_POINT('',(0.,-7.,25.));
#7973=CARTESIAN_POINT('',(0.,-7.,25.));
#7974=CARTESIAN_POINT('Origin',(0.,-7.,15.));
#7975=CARTESIAN_POINT('',(0.,-7.,15.));
#7976=CARTESIAN_POINT('',(0.,-7.,15.));
#7977=CARTESIAN_POINT('',(0.,-7.,15.));
#7978=CARTESIAN_POINT('Origin',(-8.41954981558864,-5.55111512312578E-15,
66.0000009834766));
#7979=CARTESIAN_POINT('',(-8.,-1.00000000000001,66.0000009834766));
#7980=CARTESIAN_POINT('Origin',(-8.,-5.55111512312578E-15,66.0000009834766));
#7981=CARTESIAN_POINT('',(-8.83909963117728,-5.55111512312578E-15,66.0000009834766));
#7982=CARTESIAN_POINT('',(-8.41954981558864,-0.500000000000006,66.0000009834766));
#7983=CARTESIAN_POINT('Origin',(-4.,-5.55111512312578E-15,66.0000009834766));
#7984=CARTESIAN_POINT('',(0.,-1.00000000000001,66.0000009834766));
#7985=CARTESIAN_POINT('Origin',(0.,-5.55111512312578E-15,66.0000009834766));
#7986=CARTESIAN_POINT('',(-4.,-1.00000000000001,66.0000009834766));
#7987=CARTESIAN_POINT('Origin',(-10.,0.,52.500000372529));
#7988=CARTESIAN_POINT('',(0.,-9.5,52.500000372529));
#7989=CARTESIAN_POINT('Origin',(0.,0.,52.500000372529));
#7990=CARTESIAN_POINT('',(-20.,-9.5,52.500000372529));
#7991=CARTESIAN_POINT('',(-10.,-9.5,52.500000372529));
#7992=CARTESIAN_POINT('Origin',(-20.,0.,52.500000372529));
#7993=CARTESIAN_POINT('Origin',(-20.,0.,52.500000372529));
#7994=CARTESIAN_POINT('Origin',(0.,12.5,0.));
#7995=CARTESIAN_POINT('',(0.,-12.5,0.));
#7996=CARTESIAN_POINT('',(0.,12.5,1.53080849893419E-15));
#7997=CARTESIAN_POINT('',(0.,-12.5,0.));
#7998=CARTESIAN_POINT('',(-64.,-12.5,0.));
#7999=CARTESIAN_POINT('',(0.,-12.5,0.));
#8000=CARTESIAN_POINT('',(-64.,12.5,1.53080849893419E-15));
#8001=CARTESIAN_POINT('',(-64.,-12.5,0.));
#8002=CARTESIAN_POINT('',(0.,12.5,1.53080849893419E-15));
#8003=CARTESIAN_POINT('Origin',(0.,12.5,15.));
#8004=CARTESIAN_POINT('',(0.,12.5,15.));
#8005=CARTESIAN_POINT('',(0.,12.5,1.53080849893419E-15));
#8006=CARTESIAN_POINT('',(-64.,12.5,15.));
#8007=CARTESIAN_POINT('',(-64.,12.5,1.53080849893419E-15));
#8008=CARTESIAN_POINT('',(0.,12.5,15.));
#8009=CARTESIAN_POINT('Origin',(0.,7.,15.));
#8010=CARTESIAN_POINT('',(0.,7.,15.));
#8011=CARTESIAN_POINT('',(0.,7.,15.));
#8012=CARTESIAN_POINT('',(0.,12.5,15.));
#8013=CARTESIAN_POINT('',(-64.,-12.5,15.));
#8014=CARTESIAN_POINT('',(-64.,-12.5,15.));
#8015=CARTESIAN_POINT('',(0.,-12.5,15.));
#8016=CARTESIAN_POINT('',(0.,-12.5,15.));
#8017=CARTESIAN_POINT('',(0.,-12.5,15.));
#8018=CARTESIAN_POINT('Origin',(0.,7.,25.));
#8019=CARTESIAN_POINT('',(0.,7.,25.));
#8020=CARTESIAN_POINT('',(0.,7.,25.));
#8021=CARTESIAN_POINT('',(0.,7.,15.));
#8022=CARTESIAN_POINT('Origin',(0.,12.5,25.));
#8023=CARTESIAN_POINT('',(0.,12.5,25.));
#8024=CARTESIAN_POINT('',(0.,12.5,25.));
#8025=CARTESIAN_POINT('',(0.,7.,25.));
#8026=CARTESIAN_POINT('Origin',(0.,12.5,30.));
#8027=CARTESIAN_POINT('',(0.,12.5,25.));
#8028=CARTESIAN_POINT('Origin',(0.,-12.5,0.));
#8029=CARTESIAN_POINT('',(0.,-12.5,0.));
#8030=CARTESIAN_POINT('',(-64.,-12.5,0.));
#8031=CARTESIAN_POINT('Origin',(0.,0.,35.0000001862645));
#8032=CARTESIAN_POINT('Origin',(-64.,0.,35.0000001862645));
#8033=CARTESIAN_POINT('',(0.,0.,0.));
#8034=CARTESIAN_POINT('Origin',(-23.2259351895987,-0.054016425456016,3.5));
#8035=CARTESIAN_POINT('',(-28.4759351895987,-0.0540164254560154,3.5));
#8036=CARTESIAN_POINT('Origin',(-23.2259351895987,-0.054016425456016,3.5));
#8037=CARTESIAN_POINT('',(-26.4759351895987,-0.0540164254560156,3.5));
#8038=CARTESIAN_POINT('Origin',(-23.2259351895987,-0.054016425456016,3.5));
#8039=CARTESIAN_POINT('Origin',(-23.2259351895987,-0.054016425456016,4.25));
#8040=CARTESIAN_POINT('',(-28.4759351895987,-0.0540164254560154,5.));
#8041=CARTESIAN_POINT('Origin',(-23.2259351895987,-0.054016425456016,5.));
#8042=CARTESIAN_POINT('',(-28.4759351895987,-0.0540164254560154,4.25));
#8043=CARTESIAN_POINT('Origin',(-23.2259351895987,-0.054016425456016,2.5));
#8044=CARTESIAN_POINT('',(-26.4759351895987,-0.0540164254560156,0.));
#8045=CARTESIAN_POINT('',(-26.4759351895987,-0.0540164254560156,2.5));
#8046=CARTESIAN_POINT('Origin',(-23.2259351895987,-0.054016425456016,0.));
#8047=CARTESIAN_POINT('Origin',(14.7740648104013,-0.054016425456016,3.5));
#8048=CARTESIAN_POINT('',(9.52406481040134,-0.0540164254560154,3.5));
#8049=CARTESIAN_POINT('Origin',(14.7740648104013,-0.054016425456016,3.5));
#8050=CARTESIAN_POINT('',(11.5240648104013,-0.0540164254560156,3.5));
#8051=CARTESIAN_POINT('Origin',(14.7740648104013,-0.054016425456016,3.5));
#8052=CARTESIAN_POINT('Origin',(14.7740648104013,-0.054016425456016,4.25));
#8053=CARTESIAN_POINT('',(9.52406481040134,-0.0540164254560154,5.));
#8054=CARTESIAN_POINT('Origin',(14.7740648104013,-0.054016425456016,5.));
#8055=CARTESIAN_POINT('',(9.52406481040134,-0.0540164254560154,4.25));
#8056=CARTESIAN_POINT('Origin',(14.7740648104013,-0.054016425456016,2.5));
#8057=CARTESIAN_POINT('',(11.5240648104013,-0.0540164254560156,0.));
#8058=CARTESIAN_POINT('',(11.5240648104013,-0.0540164254560156,2.5));
#8059=CARTESIAN_POINT('Origin',(14.7740648104013,-0.054016425456016,0.));
#8060=CARTESIAN_POINT('Origin',(-4.22593518959866,-2.55401642545602,0.));
#8061=CARTESIAN_POINT('',(30.7740648104013,-25.054016425456,0.));
#8062=CARTESIAN_POINT('',(-39.2259351895987,-25.054016425456,0.));
#8063=CARTESIAN_POINT('',(30.7740648104013,-25.054016425456,0.));
#8064=CARTESIAN_POINT('',(-39.2259351895987,19.945983574544,0.));
#8065=CARTESIAN_POINT('',(-39.2259351895987,-25.054016425456,0.));
#8066=CARTESIAN_POINT('',(30.7740648104013,19.945983574544,0.));
#8067=CARTESIAN_POINT('',(-39.2259351895987,19.945983574544,0.));
#8068=CARTESIAN_POINT('',(30.7740648104013,19.945983574544,0.));
#8069=CARTESIAN_POINT('Origin',(-39.2259351895987,19.945983574544,0.));
#8070=CARTESIAN_POINT('',(-39.2259351895987,-25.054016425456,5.));
#8071=CARTESIAN_POINT('',(-39.2259351895987,-25.054016425456,0.));
#8072=CARTESIAN_POINT('',(-39.2259351895987,19.945983574544,5.));
#8073=CARTESIAN_POINT('',(-39.2259351895987,-25.054016425456,5.));
#8074=CARTESIAN_POINT('',(-39.2259351895987,19.945983574544,0.));
#8075=CARTESIAN_POINT('Origin',(30.7740648104013,19.945983574544,0.));
#8076=CARTESIAN_POINT('',(30.7740648104013,19.945983574544,5.));
#8077=CARTESIAN_POINT('',(-39.2259351895987,19.945983574544,5.));
#8078=CARTESIAN_POINT('',(30.7740648104013,19.945983574544,0.));
#8079=CARTESIAN_POINT('Origin',(30.7740648104013,-25.054016425456,0.));
#8080=CARTESIAN_POINT('',(30.7740648104013,-25.054016425456,5.));
#8081=CARTESIAN_POINT('',(30.7740648104013,19.945983574544,5.));
#8082=CARTESIAN_POINT('',(30.7740648104013,-25.054016425456,0.));
#8083=CARTESIAN_POINT('Origin',(-39.2259351895987,-25.054016425456,0.));
#8084=CARTESIAN_POINT('',(30.7740648104013,-25.054016425456,5.));
#8085=CARTESIAN_POINT('Origin',(-4.22593518959866,-2.55401642545602,5.));
#8086=CARTESIAN_POINT('',(0.,0.,0.));
#8087=CARTESIAN_POINT('Origin',(1.,0.,0.));
#8088=CARTESIAN_POINT('',(1.,-3.,3.67394039744206E-16));
#8089=CARTESIAN_POINT('',(1.,-3.67394039744206E-16,-3.));
#8090=CARTESIAN_POINT('Origin',(1.,0.,0.));
#8091=CARTESIAN_POINT('',(0.,-4.89858719658941E-16,-4.));
#8092=CARTESIAN_POINT('Origin',(1.,-4.89858719658941E-16,-4.));
#8093=CARTESIAN_POINT('Origin',(0.,0.,0.));
#8094=CARTESIAN_POINT('Origin',(1.,0.,0.));
#8095=CARTESIAN_POINT('Origin',(0.,0.,0.));
#8096=CARTESIAN_POINT('',(16.,-3.,-3.67394039744206E-16));
#8097=CARTESIAN_POINT('Origin',(16.,0.,0.));
#8098=CARTESIAN_POINT('',(0.,-3.,-3.67394039744206E-16));
#8099=CARTESIAN_POINT('Origin',(0.,0.,0.));
#8100=CARTESIAN_POINT('',(0.,-5.,-6.12323399573677E-16));
#8101=CARTESIAN_POINT('Origin',(0.,0.,0.));
#8102=CARTESIAN_POINT('Origin',(-3.5,-3.03108895841228,-1.75000002607703));
#8103=CARTESIAN_POINT('',(-3.5,-3.03108895841228,-1.75000002607703));
#8104=CARTESIAN_POINT('',(-3.5,0.,-3.50000005215406));
#8105=CARTESIAN_POINT('',(-3.5,-2.27331671880921,-2.18750003259629));
#8106=CARTESIAN_POINT('',(-1.5,-3.03108895841228,-1.75000002607703));
#8107=CARTESIAN_POINT('',(-3.5,-3.03108895841228,-1.75000002607703));
#8108=CARTESIAN_POINT('',(-1.5,0.,-3.50000005215406));
#8109=CARTESIAN_POINT('',(-1.5,0.,-3.50000005215406));
#8110=CARTESIAN_POINT('',(-3.5,0.,-3.50000005215406));
#8111=CARTESIAN_POINT('Origin',(-3.5,-3.03108895841228,1.75000002607703));
#8112=CARTESIAN_POINT('',(-3.5,-3.03108895841228,1.75000002607703));
#8113=CARTESIAN_POINT('',(-3.5,-3.03108895841228,0.875000013038516));
#8114=CARTESIAN_POINT('',(-1.5,-3.03108895841228,1.75000002607703));
#8115=CARTESIAN_POINT('',(-3.5,-3.03108895841228,1.75000002607703));
#8116=CARTESIAN_POINT('',(-1.5,-3.03108895841228,-1.75000002607703));
#8117=CARTESIAN_POINT('Origin',(-3.5,-1.11022302462516E-15,3.50000005215406));
#8118=CARTESIAN_POINT('',(-3.5,-8.32667268468867E-16,3.50000005215406));
#8119=CARTESIAN_POINT('',(-3.5,-0.757772239603071,3.06250004563481));
#8120=CARTESIAN_POINT('',(-1.5,-1.11022302462516E-15,3.50000005215406));
#8121=CARTESIAN_POINT('',(-3.5,-8.32667268468867E-16,3.50000005215406));
#8122=CARTESIAN_POINT('',(-1.5,-3.03108895841228,1.75000002607703));
#8123=CARTESIAN_POINT('Origin',(-3.5,3.03108895841228,1.75000002607703));
#8124=CARTESIAN_POINT('',(-3.5,3.03108895841228,1.75000002607703));
#8125=CARTESIAN_POINT('',(-3.5,2.27331671880921,2.18750003259629));
#8126=CARTESIAN_POINT('',(-1.5,3.03108895841228,1.75000002607703));
#8127=CARTESIAN_POINT('',(-3.5,3.03108895841228,1.75000002607703));
#8128=CARTESIAN_POINT('',(-1.5,-8.32667268468867E-16,3.50000005215406));
#8129=CARTESIAN_POINT('Origin',(-3.5,3.03108895841228,-1.75000002607703));
#8130=CARTESIAN_POINT('',(-3.5,3.03108895841228,-1.75000002607703));
#8131=CARTESIAN_POINT('',(-3.5,3.03108895841228,-0.875000013038515));
#8132=CARTESIAN_POINT('',(-1.5,3.03108895841228,-1.75000002607703));
#8133=CARTESIAN_POINT('',(-3.5,3.03108895841228,-1.75000002607703));
#8134=CARTESIAN_POINT('',(-1.5,3.03108895841228,1.75000002607703));
#8135=CARTESIAN_POINT('Origin',(-3.5,0.,-3.50000005215406));
#8136=CARTESIAN_POINT('',(-3.5,0.75777223960307,-3.06250004563481));
#8137=CARTESIAN_POINT('',(-1.5,3.03108895841228,-1.75000002607703));
#8138=CARTESIAN_POINT('Origin',(-1.5,0.,0.));
#8139=CARTESIAN_POINT('Origin',(-2.5,0.,0.));
#8140=CARTESIAN_POINT('',(-3.5,-4.89858719658941E-16,-4.));
#8141=CARTESIAN_POINT('Origin',(-3.5,0.,0.));
#8142=CARTESIAN_POINT('',(-2.5,-6.12323399573677E-16,-5.));
#8143=CARTESIAN_POINT('Origin',(-2.5,-4.89858719658941E-16,-4.));
#8144=CARTESIAN_POINT('',(-2.5,-5.,6.12323399573677E-16));
#8145=CARTESIAN_POINT('Origin',(-2.5,0.,0.));
#8146=CARTESIAN_POINT('Origin',(-2.5,0.,0.));
#8147=CARTESIAN_POINT('Origin',(0.,0.,0.));
#8148=CARTESIAN_POINT('',(0.,-5.,6.12323399573677E-16));
#8149=CARTESIAN_POINT('Origin',(-3.5,0.,0.));
#8150=CARTESIAN_POINT('Origin',(16.,0.,0.));
#8151=CARTESIAN_POINT('',(0.,0.,0.));
#8152=CARTESIAN_POINT('Origin',(16.7000002980232,1.49222526803142,0.));
#8153=CARTESIAN_POINT('',(16.7000002980232,1.49222526803142,6.3263942138827));
#8154=CARTESIAN_POINT('',(16.7000002980232,-0.90777473196858,6.43629901698168));
#8155=CARTESIAN_POINT('Origin',(16.7000002980232,0.,0.));
#8156=CARTESIAN_POINT('',(16.7000002980232,1.49222526803142,9.38207139972024));
#8157=CARTESIAN_POINT('',(16.7000002980232,1.49222526803142,0.));
#8158=CARTESIAN_POINT('',(16.7000002980232,-0.90777473196858,9.45652922778751));
#8159=CARTESIAN_POINT('Origin',(16.7000002980232,0.,0.));
#8160=CARTESIAN_POINT('',(16.7000002980232,-0.90777473196858,0.));
#8161=CARTESIAN_POINT('Origin',(20.0000002980232,1.49222526803142,0.));
#8162=CARTESIAN_POINT('',(20.0000002980232,1.49222526803142,6.3263942138827));
#8163=CARTESIAN_POINT('',(9.,1.49222526803142,6.3263942138827));
#8164=CARTESIAN_POINT('',(20.0000002980232,1.49222526803142,9.38207139972024));
#8165=CARTESIAN_POINT('',(20.,1.49222526803142,0.));
#8166=CARTESIAN_POINT('',(0.,1.49222526803142,9.38207139972024));
#8167=CARTESIAN_POINT('Origin',(20.0000002980232,1.49222526803142,0.));
#8168=CARTESIAN_POINT('',(16.7000002980232,1.49222526803142,-6.3263942138827));
#8169=CARTESIAN_POINT('',(20.0000002980232,1.49222526803142,-6.3263942138827));
#8170=CARTESIAN_POINT('',(9.,1.49222526803142,-6.3263942138827));
#8171=CARTESIAN_POINT('',(16.7000002980232,1.49222526803142,-9.38207139972024));
#8172=CARTESIAN_POINT('',(16.7000002980232,1.49222526803142,0.));
#8173=CARTESIAN_POINT('',(20.0000002980232,1.49222526803142,-9.38207139972024));
#8174=CARTESIAN_POINT('',(0.,1.49222526803142,-9.38207139972024));
#8175=CARTESIAN_POINT('',(20.,1.49222526803142,0.));
#8176=CARTESIAN_POINT('Origin',(16.7000002980232,-0.90777473196858,0.));
#8177=CARTESIAN_POINT('',(20.0000002980232,-0.90777473196858,6.43629901698168));
#8178=CARTESIAN_POINT('',(9.,-0.90777473196858,6.43629901698168));
#8179=CARTESIAN_POINT('',(20.0000002980232,-0.90777473196858,9.45652922778751));
#8180=CARTESIAN_POINT('',(0.,-0.90777473196858,9.45652922778751));
#8181=CARTESIAN_POINT('',(20.,-0.90777473196858,0.));
#8182=CARTESIAN_POINT('Origin',(16.7000002980232,-0.90777473196858,0.));
#8183=CARTESIAN_POINT('',(20.0000002980232,-0.90777473196858,-6.43629901698168));
#8184=CARTESIAN_POINT('',(16.7000002980232,-0.90777473196858,-6.43629901698168));
#8185=CARTESIAN_POINT('',(9.,-0.90777473196858,-6.43629901698168));
#8186=CARTESIAN_POINT('',(20.0000002980232,-0.90777473196858,-9.45652922778751));
#8187=CARTESIAN_POINT('',(20.,-0.90777473196858,0.));
#8188=CARTESIAN_POINT('',(16.7000002980232,-0.90777473196858,-9.45652922778751));
#8189=CARTESIAN_POINT('',(0.,-0.90777473196858,-9.45652922778751));
#8190=CARTESIAN_POINT('',(16.7000002980232,-0.90777473196858,0.));
#8191=CARTESIAN_POINT('Origin',(16.7000002980232,1.49222526803142,0.));
#8192=CARTESIAN_POINT('Origin',(16.7000002980232,0.,0.));
#8193=CARTESIAN_POINT('Origin',(16.7000002980232,0.,0.));
#8194=CARTESIAN_POINT('Origin',(20.,0.,0.));
#8195=CARTESIAN_POINT('',(20.0000002980232,-6.5,7.9602041944578E-16));
#8196=CARTESIAN_POINT('Origin',(20.,0.,0.));
#8197=CARTESIAN_POINT('Origin',(20.,0.,0.));
#8198=CARTESIAN_POINT('',(20.0000002980232,-9.5,-1.16341445918999E-15));
#8199=CARTESIAN_POINT('Origin',(20.,0.,0.));
#8200=CARTESIAN_POINT('Origin',(20.,0.,0.));
#8201=CARTESIAN_POINT('Origin',(20.,0.,0.));
#8202=CARTESIAN_POINT('Origin',(20.,0.,0.));
#8203=CARTESIAN_POINT('Origin',(20.,0.,0.));
#8204=CARTESIAN_POINT('Origin',(0.,0.,0.));
#8205=CARTESIAN_POINT('',(0.,-9.5,-1.16341445918999E-15));
#8206=CARTESIAN_POINT('',(0.,-9.5,-1.16341445918999E-15));
#8207=CARTESIAN_POINT('Origin',(0.,0.,0.));
#8208=CARTESIAN_POINT('Origin',(9.,0.,0.));
#8209=CARTESIAN_POINT('',(0.,-6.5,-7.9602041944578E-16));
#8210=CARTESIAN_POINT('',(9.,-6.5,7.9602041944578E-16));
#8211=CARTESIAN_POINT('Origin',(0.,0.,0.));
#8212=CARTESIAN_POINT('Origin',(0.,0.,0.));
#8213=CARTESIAN_POINT('',(0.,0.,0.));
#8214=CARTESIAN_POINT('Origin',(0.,12.5,0.));
#8215=CARTESIAN_POINT('',(-1.25,12.5,3.3));
#8216=CARTESIAN_POINT('Origin',(0.,12.5,3.3));
#8217=CARTESIAN_POINT('',(-1.25,12.5,0.));
#8218=CARTESIAN_POINT('',(-1.25,12.5,0.));
#8219=CARTESIAN_POINT('Origin',(0.,12.5,0.));
#8220=CARTESIAN_POINT('Origin',(0.,0.,0.));
#8221=CARTESIAN_POINT('',(0.,5.00000007450581,0.));
#8222=CARTESIAN_POINT('',(-6.12323408698006E-16,-5.00000007450581,0.));
#8223=CARTESIAN_POINT('Origin',(0.,0.,0.));
#8224=CARTESIAN_POINT('',(0.,5.00000007450581,3.3));
#8225=CARTESIAN_POINT('',(0.,5.00000007450581,0.));
#8226=CARTESIAN_POINT('',(-5.55111512312578E-16,-5.00000007450581,3.3));
#8227=CARTESIAN_POINT('Origin',(0.,0.,3.3));
#8228=CARTESIAN_POINT('',(-6.12323408698006E-16,-5.00000007450581,0.));
#8229=CARTESIAN_POINT('Origin',(12.6491106053323,-5.00000007450581,0.));
#8230=CARTESIAN_POINT('',(12.6491106053323,-5.00000007450581,0.));
#8231=CARTESIAN_POINT('',(0.,-5.00000007450581,0.));
#8232=CARTESIAN_POINT('',(12.6491106053323,-5.00000007450581,3.3));
#8233=CARTESIAN_POINT('',(0.,-5.00000007450581,3.3));
#8234=CARTESIAN_POINT('',(12.6491106053323,-5.00000007450581,0.));
#8235=CARTESIAN_POINT('Origin',(12.6491106053323,-6.0000000745058,0.));
#8236=CARTESIAN_POINT('',(13.5526185057132,-6.42857150839907,0.));
#8237=CARTESIAN_POINT('Origin',(12.6491106053323,-6.0000000745058,0.));
#8238=CARTESIAN_POINT('',(13.5526185057132,-6.42857150839907,3.3));
#8239=CARTESIAN_POINT('Origin',(12.6491106053323,-6.0000000745058,3.3));
#8240=CARTESIAN_POINT('',(13.5526185057132,-6.42857150839907,0.));
#8241=CARTESIAN_POINT('Origin',(0.,0.,0.));
#8242=CARTESIAN_POINT('',(13.5526185057132,6.42857150839908,0.));
#8243=CARTESIAN_POINT('Origin',(0.,0.,0.));
#8244=CARTESIAN_POINT('',(13.5526185057132,6.42857150839908,3.3));
#8245=CARTESIAN_POINT('Origin',(0.,0.,3.3));
#8246=CARTESIAN_POINT('',(13.5526185057132,6.42857150839908,0.));
#8247=CARTESIAN_POINT('Origin',(12.6491106053323,6.00000007450581,0.));
#8248=CARTESIAN_POINT('',(12.6491106053323,5.00000007450581,0.));
#8249=CARTESIAN_POINT('Origin',(12.6491106053323,6.00000007450581,0.));
#8250=CARTESIAN_POINT('',(12.6491106053323,5.00000007450581,3.3));
#8251=CARTESIAN_POINT('Origin',(12.6491106053323,6.00000007450581,3.3));
#8252=CARTESIAN_POINT('',(12.6491106053323,5.00000007450581,0.));
#8253=CARTESIAN_POINT('Origin',(0.,5.00000007450581,0.));
#8254=CARTESIAN_POINT('',(0.,5.00000007450581,0.));
#8255=CARTESIAN_POINT('',(0.,5.00000007450581,3.3));
#8256=CARTESIAN_POINT('Origin',(-0.675444697333845,0.,3.3));
#8257=CARTESIAN_POINT('Origin',(-0.675444697333845,0.,0.));
#8258=CARTESIAN_POINT('',(0.,0.,0.));
#8259=CARTESIAN_POINT('Origin',(0.,0.35,-1.86748493969831));
#8260=CARTESIAN_POINT('',(0.,0.35,-1.86748493969831));
#8261=CARTESIAN_POINT('',(0.,0.35,1.86748493969831));
#8262=CARTESIAN_POINT('',(0.,0.35,-0.933742469849155));
#8263=CARTESIAN_POINT('',(0.5,0.35,-1.86748493969831));
#8264=CARTESIAN_POINT('',(0.,0.35,-1.86748493969831));
#8265=CARTESIAN_POINT('',(0.5,0.35,1.86748493969831));
#8266=CARTESIAN_POINT('',(0.5,0.35,0.));
#8267=CARTESIAN_POINT('',(0.,0.35,1.86748493969831));
#8268=CARTESIAN_POINT('Origin',(0.,-0.35,1.86748493969831));
#8269=CARTESIAN_POINT('',(0.,-0.35,1.86748493969831));
#8270=CARTESIAN_POINT('',(0.,-0.35,-1.86748493969831));
#8271=CARTESIAN_POINT('',(0.,-0.35,0.933742469849155));
#8272=CARTESIAN_POINT('',(0.5,-0.35,1.86748493969831));
#8273=CARTESIAN_POINT('',(0.,-0.35,1.86748493969831));
#8274=CARTESIAN_POINT('',(0.5,-0.35,-1.86748493969831));
#8275=CARTESIAN_POINT('',(0.5,-0.35,0.));
#8276=CARTESIAN_POINT('',(0.,-0.35,-1.86748493969831));
#8277=CARTESIAN_POINT('Origin',(0.5,0.,0.));
#8278=CARTESIAN_POINT('Origin',(0.5,0.,0.));
#8279=CARTESIAN_POINT('Origin',(0.5,0.,0.));
#8280=CARTESIAN_POINT('Origin',(0.,0.,0.));
#8281=CARTESIAN_POINT('',(0.,-1.9,-2.32682891837997E-16));
#8282=CARTESIAN_POINT('Origin',(0.,0.,0.));
#8283=CARTESIAN_POINT('Origin',(0.,0.,0.));
#8284=CARTESIAN_POINT('Origin',(0.,0.,0.));
#8285=CARTESIAN_POINT('Origin',(0.,0.,0.));
#8286=CARTESIAN_POINT('Origin',(1.3,0.,0.));
#8287=CARTESIAN_POINT('',(11.3,-1.,-1.22464679914735E-16));
#8288=CARTESIAN_POINT('Origin',(11.3,0.,0.));
#8289=CARTESIAN_POINT('',(1.3,-1.,-1.22464679914735E-16));
#8290=CARTESIAN_POINT('',(1.3,-1.,-1.22464679914735E-16));
#8291=CARTESIAN_POINT('Origin',(1.3,0.,0.));
#8292=CARTESIAN_POINT('Origin',(11.3,0.,0.));
#8293=CARTESIAN_POINT('Origin',(0.,0.,0.));
#8294=CARTESIAN_POINT('',(1.3,-1.9,-2.32682891837997E-16));
#8295=CARTESIAN_POINT('Origin',(1.3,0.,0.));
#8296=CARTESIAN_POINT('',(0.,-1.9,-2.32682891837997E-16));
#8297=CARTESIAN_POINT('Origin',(1.3,0.,0.));
#8298=CARTESIAN_POINT('',(0.,0.,0.));
#8299=CARTESIAN_POINT('Origin',(-25.,0.,0.));
#8300=CARTESIAN_POINT('',(-26.5,-9.79717439317883E-16,-8.));
#8301=CARTESIAN_POINT('Origin',(-26.5,0.,0.));
#8302=CARTESIAN_POINT('',(-25.,-1.16341445918999E-15,-9.5));
#8303=CARTESIAN_POINT('Origin',(-25.,-9.79717439317883E-16,-8.));
#8304=CARTESIAN_POINT('',(-25.,9.5,-1.16341445918999E-15));
#8305=CARTESIAN_POINT('Origin',(-25.,0.,0.));
#8306=CARTESIAN_POINT('Origin',(-25.,0.,0.));
#8307=CARTESIAN_POINT('Origin',(-6.5,0.,0.));
#8308=CARTESIAN_POINT('',(-19.7496152242889,9.5,-1.16341445918999E-15));
#8309=CARTESIAN_POINT('',(-6.5,9.5,-1.16341445918999E-15));
#8310=CARTESIAN_POINT('',(-19.7496152242889,-1.16341445918999E-15,9.5));
#8311=CARTESIAN_POINT('Origin',(-19.7496152242889,0.,0.));
#8312=CARTESIAN_POINT('Origin',(-19.7496152242889,0.,0.));
#8313=CARTESIAN_POINT('Origin',(-26.5,0.,0.));
#8314=CARTESIAN_POINT('Origin',(-16.5,0.,0.));
#8315=CARTESIAN_POINT('',(-13.2503847757111,9.5,1.16341445918999E-15));
#8316=CARTESIAN_POINT('',(-13.2503847757111,-1.16341445918999E-15,9.5));
#8317=CARTESIAN_POINT('Origin',(-13.2503847757111,0.,0.));
#8318=CARTESIAN_POINT('Origin',(-13.2503847757111,0.,0.));
#8319=CARTESIAN_POINT('Origin',(-16.5,-1.46957618087521E-15,12.0000001788139));
#8320=CARTESIAN_POINT('Origin',(-6.5,0.,0.));
#8321=CARTESIAN_POINT('',(-6.5,9.5,-1.16341445918999E-15));
#8322=CARTESIAN_POINT('',(-6.5,9.5,-1.16341445918999E-15));
#8323=CARTESIAN_POINT('Origin',(-6.5,0.,0.));
#8324=CARTESIAN_POINT('Origin',(-6.5,0.,0.));
#8325=CARTESIAN_POINT('',(-6.5,6.5,-7.96020419445779E-16));
#8326=CARTESIAN_POINT('Origin',(-6.5,0.,0.));
#8327=CARTESIAN_POINT('Origin',(0.,0.,0.));
#8328=CARTESIAN_POINT('',(0.,6.5,-7.96020419445779E-16));
#8329=CARTESIAN_POINT('',(0.,6.5,-7.96020419445779E-16));
#8330=CARTESIAN_POINT('Origin',(0.,0.,0.));
#8331=CARTESIAN_POINT('Origin',(113.5,0.,0.));
#8332=CARTESIAN_POINT('',(113.5,-6.50000009685755,-7.96020431307408E-16));
#8333=CARTESIAN_POINT('Origin',(113.5,0.,0.));
#8334=CARTESIAN_POINT('',(113.5,-4.75,-5.81707229594993E-16));
#8335=CARTESIAN_POINT('Origin',(113.5,0.,0.));
#8336=CARTESIAN_POINT('Origin',(113.5,0.,0.));
#8337=CARTESIAN_POINT('',(133.5,-6.50000009685755,-7.96020431307408E-16));
#8338=CARTESIAN_POINT('Origin',(133.5,0.,0.));
#8339=CARTESIAN_POINT('',(113.5,-6.50000009685755,-7.96020431307408E-16));
#8340=CARTESIAN_POINT('Origin',(133.5,0.,0.));
#8341=CARTESIAN_POINT('Origin',(110.,0.,0.));
#8342=CARTESIAN_POINT('',(110.,-4.75,-5.81707229594993E-16));
#8343=CARTESIAN_POINT('',(110.,-4.75,-5.81707229594993E-16));
#8344=CARTESIAN_POINT('Origin',(110.,0.,0.));
#8345=CARTESIAN_POINT('Origin',(100.5,0.,0.));
#8346=CARTESIAN_POINT('',(110.,-6.5,-7.9602041944578E-16));
#8347=CARTESIAN_POINT('Origin',(110.,0.,0.));
#8348=CARTESIAN_POINT('',(100.5,-6.5,-7.9602041944578E-16));
#8349=CARTESIAN_POINT('',(100.5,-6.5,-7.9602041944578E-16));
#8350=CARTESIAN_POINT('Origin',(100.5,0.,0.));
#8351=CARTESIAN_POINT('Origin',(110.,0.,0.));
#8352=CARTESIAN_POINT('Origin',(0.,0.,0.));
#8353=CARTESIAN_POINT('',(100.5,-8.,-9.79717439317883E-16));
#8354=CARTESIAN_POINT('Origin',(100.5,0.,0.));
#8355=CARTESIAN_POINT('',(0.,-8.,-9.79717439317883E-16));
#8356=CARTESIAN_POINT('',(0.,-8.,-9.79717439317883E-16));
#8357=CARTESIAN_POINT('Origin',(0.,0.,0.));
#8358=CARTESIAN_POINT('Origin',(100.5,0.,0.));
#8359=CARTESIAN_POINT('Origin',(0.,0.,0.));
#8360=CARTESIAN_POINT('',(0.,0.,0.));
#8361=CARTESIAN_POINT('Origin',(27.9999995231628,0.,0.));
#8362=CARTESIAN_POINT('',(27.9999995231628,4.4,0.));
#8363=CARTESIAN_POINT('',(27.9999995231628,0.,0.));
#8364=CARTESIAN_POINT('',(27.9999995231628,4.4,0.));
#8365=CARTESIAN_POINT('',(27.9999995231628,4.4,5.6));
#8366=CARTESIAN_POINT('',(27.9999995231628,4.4,0.));
#8367=CARTESIAN_POINT('',(27.9999995231628,0.,5.6));
#8368=CARTESIAN_POINT('',(27.9999995231628,4.4,5.6));
#8369=CARTESIAN_POINT('',(27.9999995231628,0.,0.));
#8370=CARTESIAN_POINT('Origin',(0.,0.,0.));
#8371=CARTESIAN_POINT('',(0.,0.,0.));
#8372=CARTESIAN_POINT('',(0.,0.,0.));
#8373=CARTESIAN_POINT('',(0.,0.,5.6));
#8374=CARTESIAN_POINT('',(0.,0.,5.6));
#8375=CARTESIAN_POINT('',(0.,0.,0.));
#8376=CARTESIAN_POINT('Origin',(0.,8.6,0.));
#8377=CARTESIAN_POINT('',(0.,8.6,0.));
#8378=CARTESIAN_POINT('',(0.,8.6,0.));
#8379=CARTESIAN_POINT('',(0.,8.6,5.6));
#8380=CARTESIAN_POINT('',(0.,8.6,5.6));
#8381=CARTESIAN_POINT('',(0.,8.6,0.));
#8382=CARTESIAN_POINT('Origin',(60.,8.6,0.));
#8383=CARTESIAN_POINT('',(60.,8.6,0.));
#8384=CARTESIAN_POINT('',(60.,8.6,0.));
#8385=CARTESIAN_POINT('',(60.,8.6,5.6));
#8386=CARTESIAN_POINT('',(60.,8.6,5.6));
#8387=CARTESIAN_POINT('',(60.,8.6,0.));
#8388=CARTESIAN_POINT('Origin',(60.,0.,0.));
#8389=CARTESIAN_POINT('',(60.,0.,0.));
#8390=CARTESIAN_POINT('',(60.,0.,0.));
#8391=CARTESIAN_POINT('',(60.,0.,5.6));
#8392=CARTESIAN_POINT('',(60.,0.,5.6));
#8393=CARTESIAN_POINT('',(60.,0.,0.));
#8394=CARTESIAN_POINT('Origin',(32.0000004768372,0.,0.));
#8395=CARTESIAN_POINT('',(32.0000004768372,0.,0.));
#8396=CARTESIAN_POINT('',(32.0000004768372,0.,0.));
#8397=CARTESIAN_POINT('',(32.0000004768372,0.,5.6));
#8398=CARTESIAN_POINT('',(32.0000004768372,0.,5.6));
#8399=CARTESIAN_POINT('',(32.0000004768372,0.,0.));
#8400=CARTESIAN_POINT('Origin',(32.0000004768372,4.4,0.));
#8401=CARTESIAN_POINT('',(32.0000004768372,4.4,0.));
#8402=CARTESIAN_POINT('',(32.0000004768372,4.4,0.));
#8403=CARTESIAN_POINT('',(32.0000004768372,4.4,5.6));
#8404=CARTESIAN_POINT('',(32.0000004768372,4.4,5.6));
#8405=CARTESIAN_POINT('',(32.0000004768372,4.4,0.));
#8406=CARTESIAN_POINT('Origin',(27.9999995231628,4.4,0.));
#8407=CARTESIAN_POINT('',(27.9999995231628,4.4,0.));
#8408=CARTESIAN_POINT('',(27.9999995231628,4.4,5.6));
#8409=CARTESIAN_POINT('Origin',(30.,4.3,5.6));
#8410=CARTESIAN_POINT('Origin',(30.,4.3,0.));
#8411=CARTESIAN_POINT('',(0.,0.,0.));
#8412=CARTESIAN_POINT('',(31.47224362268,4.22593518959866,62.0540164254558));
#8413=CARTESIAN_POINT('',(32.47224362268,-19.0000000000002,62.));
#8414=CARTESIAN_POINT('',(32.47224362268,19.,62.));
#8415=CARTESIAN_POINT('',(135.61992406845,0.,7.00000000000056));
#8416=CARTESIAN_POINT('',(95.6199240684509,-4.2259354727207,62.0540164254561));
#8417=CARTESIAN_POINT('',(94.6199240684509,19.,62.));
#8418=CARTESIAN_POINT('',(94.6199240684509,-19.0000002831221,62.));
#8419=CARTESIAN_POINT('',(113.704221248627,0.,59.500000372529));
#8420=CARTESIAN_POINT('',(135.619924068451,2.74225087082414E-13,60.5000009834766));
#8421=CARTESIAN_POINT('',(140.219924068451,-1.49835517711341E-13,73.0000009834766));
#8422=CARTESIAN_POINT('',(252.661528587341,-3.73034936274053E-12,59.500000372529));
#8423=CARTESIAN_POINT('',(46.749804019928,12.6,20.4510353207588));
#8424=UNCERTAINTY_MEASURE_WITH_UNIT(LENGTH_MEASURE(0.01),#8446,
'DISTANCE_ACCURACY_VALUE',
'Maximum model space distance between geometric entities at asserted c
onnectivities');
#8425=UNCERTAINTY_MEASURE_WITH_UNIT(LENGTH_MEASURE(0.01),#8446,
'DISTANCE_ACCURACY_VALUE',
'Maximum model space distance between geometric entities at asserted c
onnectivities');
#8426=UNCERTAINTY_MEASURE_WITH_UNIT(LENGTH_MEASURE(0.01),#8446,
'DISTANCE_ACCURACY_VALUE',
'Maximum model space distance between geometric entities at asserted c
onnectivities');
#8427=UNCERTAINTY_MEASURE_WITH_UNIT(LENGTH_MEASURE(0.01),#8446,
'DISTANCE_ACCURACY_VALUE',
'Maximum model space distance between geometric entities at asserted c
onnectivities');
#8428=UNCERTAINTY_MEASURE_WITH_UNIT(LENGTH_MEASURE(0.01),#8446,
'DISTANCE_ACCURACY_VALUE',
'Maximum model space distance between geometric entities at asserted c
onnectivities');
#8429=UNCERTAINTY_MEASURE_WITH_UNIT(LENGTH_MEASURE(0.01),#8446,
'DISTANCE_ACCURACY_VALUE',
'Maximum model space distance between geometric entities at asserted c
onnectivities');
#8430=UNCERTAINTY_MEASURE_WITH_UNIT(LENGTH_MEASURE(0.01),#8446,
'DISTANCE_ACCURACY_VALUE',
'Maximum model space distance between geometric entities at asserted c
onnectivities');
#8431=UNCERTAINTY_MEASURE_WITH_UNIT(LENGTH_MEASURE(0.01),#8446,
'DISTANCE_ACCURACY_VALUE',
'Maximum model space distance between geometric entities at asserted c
onnectivities');
#8432=UNCERTAINTY_MEASURE_WITH_UNIT(LENGTH_MEASURE(0.01),#8446,
'DISTANCE_ACCURACY_VALUE',
'Maximum model space distance between geometric entities at asserted c
onnectivities');
#8433=UNCERTAINTY_MEASURE_WITH_UNIT(LENGTH_MEASURE(0.01),#8446,
'DISTANCE_ACCURACY_VALUE',
'Maximum model space distance between geometric entities at asserted c
onnectivities');
#8434=UNCERTAINTY_MEASURE_WITH_UNIT(LENGTH_MEASURE(0.01),#8446,
'DISTANCE_ACCURACY_VALUE',
'Maximum model space distance between geometric entities at asserted c
onnectivities');
#8435=(
GEOMETRIC_REPRESENTATION_CONTEXT(3)
GLOBAL_UNCERTAINTY_ASSIGNED_CONTEXT((#8424))
GLOBAL_UNIT_ASSIGNED_CONTEXT((#8446,#8448,#8449))
REPRESENTATION_CONTEXT('','3D')
);
#8436=(
GEOMETRIC_REPRESENTATION_CONTEXT(3)
GLOBAL_UNCERTAINTY_ASSIGNED_CONTEXT((#8425))
GLOBAL_UNIT_ASSIGNED_CONTEXT((#8446,#8448,#8449))
REPRESENTATION_CONTEXT('','3D')
);
#8437=(
GEOMETRIC_REPRESENTATION_CONTEXT(3)
GLOBAL_UNCERTAINTY_ASSIGNED_CONTEXT((#8426))
GLOBAL_UNIT_ASSIGNED_CONTEXT((#8446,#8448,#8449))
REPRESENTATION_CONTEXT('','3D')
);
#8438=(
GEOMETRIC_REPRESENTATION_CONTEXT(3)
GLOBAL_UNCERTAINTY_ASSIGNED_CONTEXT((#8427))
GLOBAL_UNIT_ASSIGNED_CONTEXT((#8446,#8448,#8449))
REPRESENTATION_CONTEXT('','3D')
);
#8439=(
GEOMETRIC_REPRESENTATION_CONTEXT(3)
GLOBAL_UNCERTAINTY_ASSIGNED_CONTEXT((#8428))
GLOBAL_UNIT_ASSIGNED_CONTEXT((#8446,#8448,#8449))
REPRESENTATION_CONTEXT('','3D')
);
#8440=(
GEOMETRIC_REPRESENTATION_CONTEXT(3)
GLOBAL_UNCERTAINTY_ASSIGNED_CONTEXT((#8429))
GLOBAL_UNIT_ASSIGNED_CONTEXT((#8446,#8448,#8449))
REPRESENTATION_CONTEXT('','3D')
);
#8441=(
GEOMETRIC_REPRESENTATION_CONTEXT(3)
GLOBAL_UNCERTAINTY_ASSIGNED_CONTEXT((#8430))
GLOBAL_UNIT_ASSIGNED_CONTEXT((#8446,#8448,#8449))
REPRESENTATION_CONTEXT('','3D')
);
#8442=(
GEOMETRIC_REPRESENTATION_CONTEXT(3)
GLOBAL_UNCERTAINTY_ASSIGNED_CONTEXT((#8431))
GLOBAL_UNIT_ASSIGNED_CONTEXT((#8446,#8448,#8449))
REPRESENTATION_CONTEXT('','3D')
);
#8443=(
GEOMETRIC_REPRESENTATION_CONTEXT(3)
GLOBAL_UNCERTAINTY_ASSIGNED_CONTEXT((#8432))
GLOBAL_UNIT_ASSIGNED_CONTEXT((#8446,#8448,#8449))
REPRESENTATION_CONTEXT('','3D')
);
#8444=(
GEOMETRIC_REPRESENTATION_CONTEXT(3)
GLOBAL_UNCERTAINTY_ASSIGNED_CONTEXT((#8433))
GLOBAL_UNIT_ASSIGNED_CONTEXT((#8446,#8448,#8449))
REPRESENTATION_CONTEXT('','3D')
);
#8445=(
GEOMETRIC_REPRESENTATION_CONTEXT(3)
GLOBAL_UNCERTAINTY_ASSIGNED_CONTEXT((#8434))
GLOBAL_UNIT_ASSIGNED_CONTEXT((#8446,#8448,#8449))
REPRESENTATION_CONTEXT('','3D')
);
#8446=(
LENGTH_UNIT()
NAMED_UNIT(*)
SI_UNIT(.MILLI.,.METRE.)
);
#8447=(
LENGTH_UNIT()
NAMED_UNIT(*)
SI_UNIT($,.METRE.)
);
#8448=(
NAMED_UNIT(*)
PLANE_ANGLE_UNIT()
SI_UNIT($,.RADIAN.)
);
#8449=(
NAMED_UNIT(*)
SI_UNIT($,.STERADIAN.)
SOLID_ANGLE_UNIT()
);
#8450=SHAPE_DEFINITION_REPRESENTATION(#8460,#8483);
#8451=SHAPE_DEFINITION_REPRESENTATION(#8461,#8484);
#8452=SHAPE_DEFINITION_REPRESENTATION(#8462,#8485);
#8453=SHAPE_DEFINITION_REPRESENTATION(#8463,#8486);
#8454=SHAPE_DEFINITION_REPRESENTATION(#8464,#8487);
#8455=SHAPE_DEFINITION_REPRESENTATION(#8465,#8488);
#8456=SHAPE_DEFINITION_REPRESENTATION(#8466,#8489);
#8457=SHAPE_DEFINITION_REPRESENTATION(#8467,#8490);
#8458=SHAPE_DEFINITION_REPRESENTATION(#8468,#8491);
#8459=SHAPE_DEFINITION_REPRESENTATION(#8469,#8492);
#8460=PRODUCT_DEFINITION_SHAPE('',$,#8494);
#8461=PRODUCT_DEFINITION_SHAPE('',$,#8495);
#8462=PRODUCT_DEFINITION_SHAPE('',$,#8496);
#8463=PRODUCT_DEFINITION_SHAPE('',$,#8497);
#8464=PRODUCT_DEFINITION_SHAPE('',$,#8498);
#8465=PRODUCT_DEFINITION_SHAPE('',$,#8499);
#8466=PRODUCT_DEFINITION_SHAPE('',$,#8500);
#8467=PRODUCT_DEFINITION_SHAPE('',$,#8501);
#8468=PRODUCT_DEFINITION_SHAPE('',$,#8502);
#8469=PRODUCT_DEFINITION_SHAPE('',$,#8503);
#8470=PRODUCT_DEFINITION_SHAPE($,$,#50);
#8471=PRODUCT_DEFINITION_SHAPE($,$,#51);
#8472=PRODUCT_DEFINITION_SHAPE($,$,#52);
#8473=PRODUCT_DEFINITION_SHAPE($,$,#53);
#8474=PRODUCT_DEFINITION_SHAPE($,$,#54);
#8475=PRODUCT_DEFINITION_SHAPE($,$,#55);
#8476=PRODUCT_DEFINITION_SHAPE($,$,#56);
#8477=PRODUCT_DEFINITION_SHAPE($,$,#57);
#8478=PRODUCT_DEFINITION_SHAPE($,$,#58);
#8479=PRODUCT_DEFINITION_SHAPE($,$,#59);
#8480=PRODUCT_DEFINITION_SHAPE($,$,#60);
#8481=PRODUCT_DEFINITION_SHAPE($,$,#61);
#8482=PRODUCT_DEFINITION_SHAPE($,$,#62);
#8483=SHAPE_REPRESENTATION('',(#4111,#4500,#4501,#4502,#4503,#4504,#4505,
#4506,#4507,#4508,#4509,#4510,#4511,#4512),#8435);
#8484=SHAPE_REPRESENTATION('',(#4112),#8436);
#8485=SHAPE_REPRESENTATION('',(#4284),#8437);
#8486=SHAPE_REPRESENTATION('',(#4344),#8438);
#8487=SHAPE_REPRESENTATION('',(#4365),#8439);
#8488=SHAPE_REPRESENTATION('',(#4390),#8440);
#8489=SHAPE_REPRESENTATION('',(#4414),#8441);
#8490=SHAPE_REPRESENTATION('',(#4434),#8442);
#8491=SHAPE_REPRESENTATION('',(#4452),#8443);
#8492=SHAPE_REPRESENTATION('',(#4489),#8444);
#8493=PRODUCT_DEFINITION_CONTEXT('part definition',#8525,'design');
#8494=PRODUCT_DEFINITION('2026-10-05-17-21-31-728','MAS-612',#8504,#8493);
#8495=PRODUCT_DEFINITION('2026-10-05-16-34-41-040','Configuration 1',#8505,
#8493);
#8496=PRODUCT_DEFINITION('2026-10-05-01-11-38-185','Configuration 1',#8506,
#8493);
#8497=PRODUCT_DEFINITION('2026-10-04-20-12-21-923','Configuration 1',#8507,
#8493);
#8498=PRODUCT_DEFINITION('2026-10-05-11-50-53-123','PO10',#8508,#8493);
#8499=PRODUCT_DEFINITION('2026-10-05-11-51-15-560','PO7',#8509,#8493);
#8500=PRODUCT_DEFINITION('2026-10-05-11-51-25-783','PO8',#8510,#8493);
#8501=PRODUCT_DEFINITION('2026-10-05-11-51-05-164','PO12',#8511,#8493);
#8502=PRODUCT_DEFINITION('2026-10-05-11-51-15-581','PO4',#8512,#8493);
#8503=PRODUCT_DEFINITION('2026-10-05-11-51-31-362','PO9',#8513,#8493);
#8504=PRODUCT_DEFINITION_FORMATION('',$,#8527);
#8505=PRODUCT_DEFINITION_FORMATION('',$,#8528);
#8506=PRODUCT_DEFINITION_FORMATION('',$,#8529);
#8507=PRODUCT_DEFINITION_FORMATION('',$,#8530);
#8508=PRODUCT_DEFINITION_FORMATION('',$,#8531);
#8509=PRODUCT_DEFINITION_FORMATION('',$,#8532);
#8510=PRODUCT_DEFINITION_FORMATION('',$,#8533);
#8511=PRODUCT_DEFINITION_FORMATION('',$,#8534);
#8512=PRODUCT_DEFINITION_FORMATION('',$,#8535);
#8513=PRODUCT_DEFINITION_FORMATION('',$,#8536);
#8514=PRODUCT_RELATED_PRODUCT_CATEGORY('MAS-612','MAS-612',(#8527));
#8515=PRODUCT_RELATED_PRODUCT_CATEGORY('Configuration 1',
'Configuration 1',(#8528));
#8516=PRODUCT_RELATED_PRODUCT_CATEGORY('Configuration 1',
'Configuration 1',(#8529));
#8517=PRODUCT_RELATED_PRODUCT_CATEGORY('Configuration 1',
'Configuration 1',(#8530));
#8518=PRODUCT_RELATED_PRODUCT_CATEGORY('PO10','PO10',(#8531));
#8519=PRODUCT_RELATED_PRODUCT_CATEGORY('PO7','PO7',(#8532));
#8520=PRODUCT_RELATED_PRODUCT_CATEGORY('PO8','PO8',(#8533));
#8521=PRODUCT_RELATED_PRODUCT_CATEGORY('PO12','PO12',(#8534));
#8522=PRODUCT_RELATED_PRODUCT_CATEGORY('PO4','PO4',(#8535));
#8523=PRODUCT_RELATED_PRODUCT_CATEGORY('PO9','PO9',(#8536));
#8524=APPLICATION_PROTOCOL_DEFINITION('international standard',
'automotive_design',2009,#8525);
#8525=APPLICATION_CONTEXT(
'Core Data for Automotive Mechanical Design Process');
#8526=PRODUCT_CONTEXT('part definition',#8525,'mechanical');
#8527=PRODUCT('2026-10-05-17-21-31-728','MAS-612',$,(#8526));
#8528=PRODUCT('2026-10-05-16-34-41-040','Configuration 1',$,(#8526));
#8529=PRODUCT('2026-10-05-01-11-38-185','Configuration 1',$,(#8526));
#8530=PRODUCT('2026-10-04-20-12-21-923','Configuration 1',$,(#8526));
#8531=PRODUCT('2026-10-05-11-50-53-123','PO10',$,(#8526));
#8532=PRODUCT('2026-10-05-11-51-15-560','PO7',$,(#8526));
#8533=PRODUCT('2026-10-05-11-51-25-783','PO8',$,(#8526));
#8534=PRODUCT('2026-10-05-11-51-05-164','PO12',$,(#8526));
#8535=PRODUCT('2026-10-05-11-51-15-581','PO4',$,(#8526));
#8536=PRODUCT('2026-10-05-11-51-31-362','PO9',$,(#8526));
#8537=PRESENTATION_STYLE_ASSIGNMENT((#8538));
#8538=SURFACE_STYLE_USAGE(.BOTH.,#8539);
#8539=SURFACE_SIDE_STYLE('',(#8540));
#8540=SURFACE_STYLE_FILL_AREA(#8541);
#8541=FILL_AREA_STYLE('Steel - Satin',(#8542));
#8542=FILL_AREA_STYLE_COLOUR('Steel - Satin',#8543);
#8543=COLOUR_RGB('Steel - Satin', 0.09019608, 0.27058824, 0.51372549);
ENDSEC;
END-ISO-10303-21;
